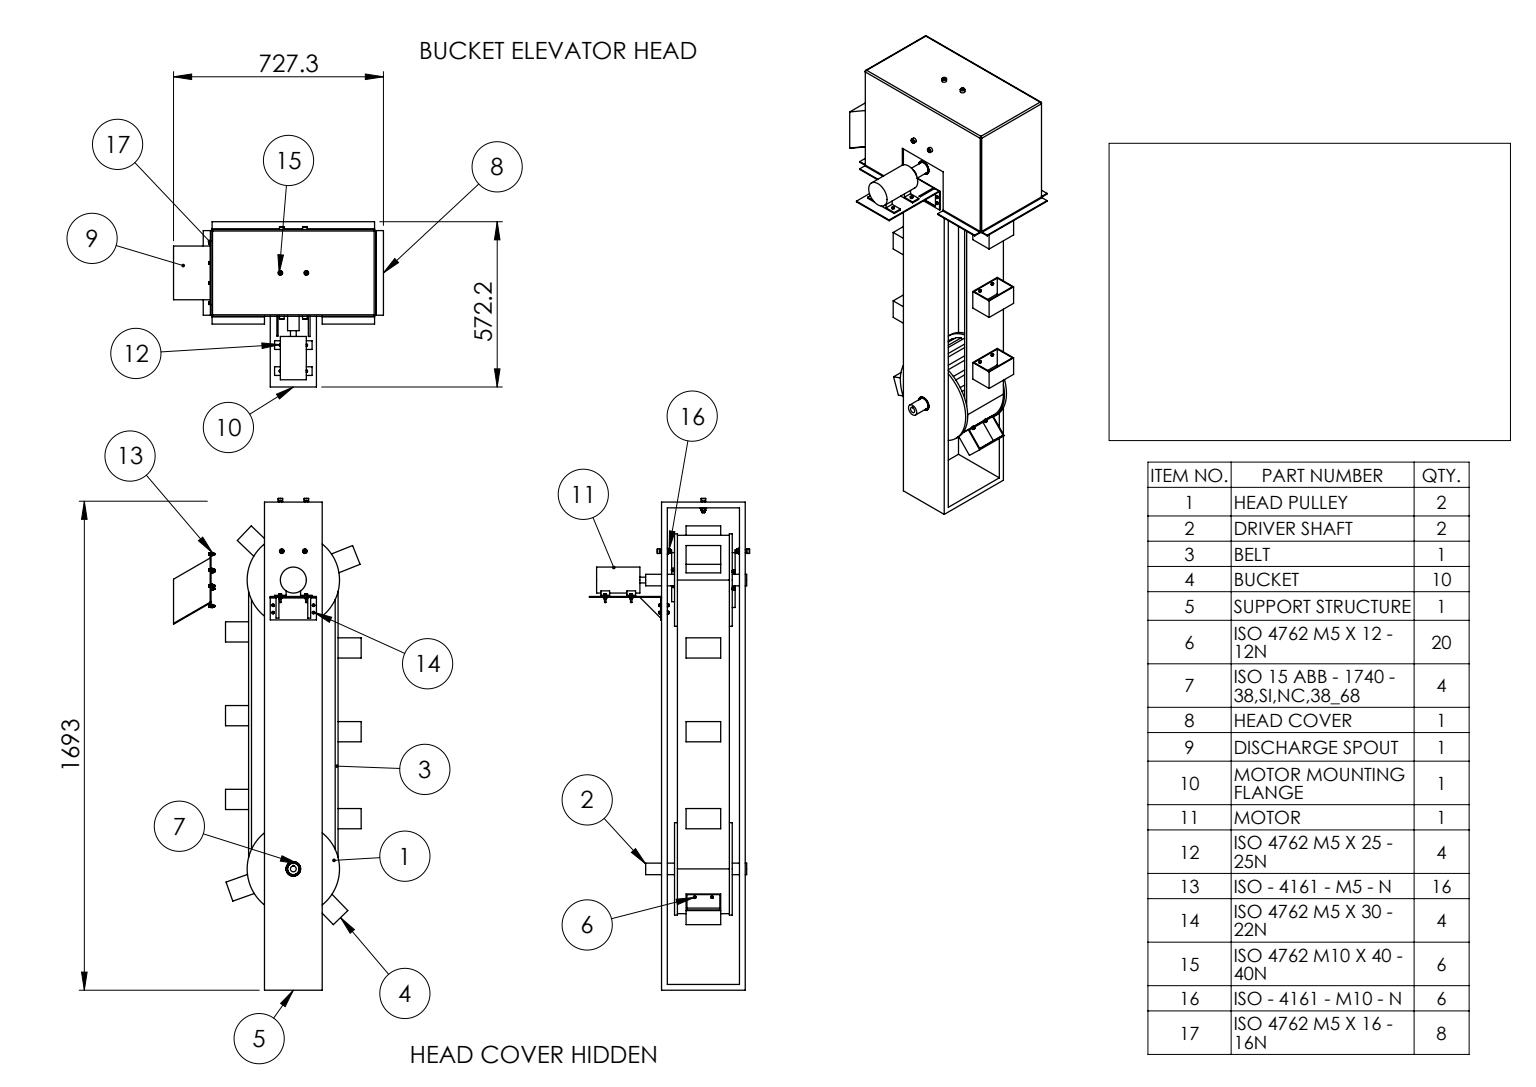
ISO-10303-21;
HEADER;
FILE_DESCRIPTION (('STEP AP214'),
    '1' );
FILE_NAME ('MAS-186',
    '2026-10-31T03:46:07',
    ( '' ),
    ( '' ),
    'SwSTEP 2.0',
    'SolidWorks 2026',
    '' );
FILE_SCHEMA (( 'AUTOMOTIVE_DESIGN' ));
ENDSEC;

DATA;
#1 = DIRECTION ( 'NONE',  ( -0.000000000000000000, -0.000000000000000000, -1.000000000000000000 ) ) ;
#2 = AXIS2_PLACEMENT_3D ( 'NONE', #6782, #12036, #15971 ) ;
#3 = VECTOR ( 'NONE', #6324, 1000.000000000000000 ) ;
#4 = CIRCLE ( 'NONE', #6942, 9.999999999999998224 ) ;
#5 = EDGE_LOOP ( 'NONE', ( #366, #3432, #8701, #5871, #3805 ) ) ;
#6 = CARTESIAN_POINT ( 'NONE',  ( 18.83467029480910071, -16.52066876451827326, 145.0000119999999697 ) ) ;
#7 = VECTOR ( 'NONE', #7349, 1000.000000000000000 ) ;
#8 = UNCERTAINTY_MEASURE_WITH_UNIT (LENGTH_MEASURE( 1.000000000000000082E-05 ), #17225, 'distance_accuracy_value', 'NONE');
#9 = CARTESIAN_POINT ( 'NONE',  ( 155.0000000000000568, -1000.000000000000000, 90.00000000000000000 ) ) ;
#10 = CARTESIAN_POINT ( 'NONE',  ( 4.000000000000000000, 2.309401076758515803, -0.4999999999999995559 ) ) ;
#11 = AXIS2_PLACEMENT_3D ( 'NONE', #10310, #5106, #19826 ) ;
#12 = VERTEX_POINT ( 'NONE', #4836 ) ;
#13 =( REPRESENTATION_RELATIONSHIP ('NONE','NONE', #10127, #5587 ) REPRESENTATION_RELATIONSHIP_WITH_TRANSFORMATION ( #17180 )SHAPE_REPRESENTATION_RELATIONSHIP( ) );
#14 = DIRECTION ( 'NONE',  ( 1.000000000000000000, -6.640089860198304064E-16, -0.000000000000000000 ) ) ;
#15 = AXIS2_PLACEMENT_3D ( 'NONE', #6057, #12994, #3756 ) ;
#16 = VECTOR ( 'NONE', #9447, 1000.000000000000114 ) ;
#17 = AXIS2_PLACEMENT_3D ( 'NONE', #8698, #6875, #2876 ) ;
#18 = CIRCLE ( 'NONE', #21621, 2.499999999999998668 ) ;
#19 = EDGE_CURVE ( 'NONE', #8380, #2021, #17168, .T. ) ;
#20 = ORIENTED_EDGE ( 'NONE', *, *, #18012, .T. ) ;
#21 = CARTESIAN_POINT ( 'NONE',  ( -31.74999999999995737, 0.000000000000000000, 4.250000000000000000 ) ) ;
#22 = EDGE_CURVE ( 'NONE', #12572, #17693, #16078, .T. ) ;
#23 = DIRECTION ( 'NONE',  ( -0.000000000000000000, -0.000000000000000000, 1.000000000000000000 ) ) ;
#24 = ORIENTED_EDGE ( 'NONE', *, *, #13771, .T. ) ;
#25 = CARTESIAN_POINT ( 'NONE',  ( -128.2695163047654319, 87.01699568756248482, -27.57873596473009670 ) ) ;
#26 = EDGE_CURVE ( 'NONE', #18313, #7126, #7119, .T. ) ;
#27 = DIRECTION ( 'NONE',  ( 0.000000000000000000, 1.177509268541832635E-16, -1.000000000000000000 ) ) ;
#28 = CARTESIAN_POINT ( 'NONE',  ( 15.24974479720505549, -1019.877690639539310, 145.0000119999999697 ) ) ;
#29 = DIRECTION ( 'NONE',  ( 0.000000000000000000, 0.7071067811865489050, 0.7071067811865462405 ) ) ;
#30 = CARTESIAN_POINT ( 'NONE',  ( -3.096526599377909417, 6.872473572140716414, 1.143494478793305063E-15 ) ) ;
#31 = EDGE_CURVE ( 'NONE', #18619, #12627, #9184, .T. ) ;
#32 = EDGE_CURVE ( 'NONE', #16311, #19722, #7366, .T. ) ;
#33 = DIRECTION ( 'NONE',  ( -1.000000000000000000, -0.000000000000000000, -0.000000000000000000 ) ) ;
#34 = EDGE_LOOP ( 'NONE', ( #18835, #10262, #758, #19921 ) ) ;
#23804 = DIRECTION ( 'NONE',  ( -1.000000000000000000, -0.000000000000000000, -0.000000000000000000 ) ) ;
#36 = CARTESIAN_POINT ( 'NONE',  ( -146.0000000000001137, -204.4690652294807478, 27.94500000000641649 ) ) ;
#37 = LINE ( 'NONE', #254, #11884 ) ;
#38 = SURFACE_SIDE_STYLE ('',( #3514 ) ) ;
#39 = VECTOR ( 'NONE', #3560, 1000.000000000000000 ) ;
#41 = ORIENTED_EDGE ( 'NONE', *, *, #15976, .F. ) ;
#40 = EDGE_LOOP ( 'NONE', ( #2219, #256, #14388 ) ) ;
#42 = DIRECTION ( 'NONE',  ( 1.000000000000000000, 0.000000000000000000, 0.000000000000000000 ) ) ;
#43 = CARTESIAN_POINT ( 'NONE',  ( 0.000000000000000000, 1.178949249685218970, 2.041999999999998483 ) ) ;
#44 = CARTESIAN_POINT ( 'NONE',  ( 280.4976310729377929, 269.6958543268122526, -146.0927021017107279 ) ) ;
#45 = VERTEX_POINT ( 'NONE', #9 ) ;
#46 = DIRECTION ( 'NONE',  ( 1.000000000000000000, -0.000000000000000000, -0.000000000000000000 ) ) ;
#47 = EDGE_LOOP ( 'NONE', ( #6115, #19407 ) ) ;
#48 = CARTESIAN_POINT ( 'NONE',  ( 80.00000000000004263, -137.9999999999999716, 3.000000000000000000 ) ) ;
#49 = ORIENTED_EDGE ( 'NONE', *, *, #7796, .F. ) ;
#50 = CARTESIAN_POINT ( 'NONE',  ( 281.4928932188134354, -129.2000000000000455, -150.2000000000013245 ) ) ;
#51 = DIRECTION ( 'NONE',  ( -0.000000000000000000, 3.469446951953613794E-15, 1.000000000000000000 ) ) ;
#52 = VERTEX_POINT ( 'NONE', #18122 ) ;
#53 = LINE ( 'NONE', #5589, #20648 ) ;
#54 = EDGE_LOOP ( 'NONE', ( #6384, #11170, #16002, #7000 ) ) ;
#55 = DIRECTION ( 'NONE',  ( 0.9289202219288174023, 0.3702799228849934510, 6.982962677686266711E-15 ) ) ;
#56 = CARTESIAN_POINT ( 'NONE',  ( 133.4872637682705090, 78.77924338079024835, 32.17229779615544771 ) ) ;
#57 = CARTESIAN_POINT ( 'NONE',  ( 3.511755186886750923, -2.826662030176382956, -3.597382984111582083 ) ) ;
#58 = DIRECTION ( 'NONE',  ( -1.000000000000000000, 0.000000000000000000, 0.000000000000000000 ) ) ;
#59 = EDGE_CURVE ( 'NONE', #14664, #1301, #12963, .T. ) ;
#60 = EDGE_CURVE ( 'NONE', #21739, #840, #11018, .T. ) ;
#61 = CARTESIAN_POINT ( 'NONE',  ( -4.204015924366189871, 1.626724848190922446, -3.610627190413390419 ) ) ;
#62 = EDGE_CURVE ( 'NONE', #22159, #2544, #22076, .T. ) ;
#63 = ORIENTED_EDGE ( 'NONE', *, *, #22259, .T. ) ;
#64 = DIRECTION ( 'NONE',  ( 0.000000000000000000, 0.000000000000000000, 1.000000000000000000 ) ) ;
#65 = CARTESIAN_POINT ( 'NONE',  ( -7.500000000000000000, 4.330127018922191873, -0.9999999999999970024 ) ) ;
#66 = CARTESIAN_POINT ( 'NONE',  ( 1.249999999999999112, -7.938566201357367902, -7.198902722707431145 ) ) ;
#67 = VERTEX_POINT ( 'NONE', #12958 ) ;
#68 = CARTESIAN_POINT ( 'NONE',  ( 281.3673618604586295, 268.0905802150185195, -147.1999999999998749 ) ) ;
#69 = CARTESIAN_POINT ( 'NONE',  ( 107.6499999999999631, -19.99999999999998934, 0.000000000000000000 ) ) ;
#70 = CARTESIAN_POINT ( 'NONE',  ( 7.499999999999999112, 0.7513028741560161539, -0.02472015219302839059 ) ) ;
#71 = DIRECTION ( 'NONE',  ( 1.000000000000000000, 0.000000000000000000, 0.000000000000000000 ) ) ;
#72 = CARTESIAN_POINT ( 'NONE',  ( 5.000000000000002665, 0.000000000000000000, -2.700000000000000622 ) ) ;
#73 = ORIENTED_EDGE ( 'NONE', *, *, #3413, .T. ) ;
#74 = CARTESIAN_POINT ( 'NONE',  ( 126.3653543294811499, 77.28387428943223370, 30.00000000000641620 ) ) ;
#75 = ORIENTED_EDGE ( 'NONE', *, *, #4902, .T. ) ;
#76 = CARTESIAN_POINT ( 'NONE',  ( 3.333333333333335702, -2.694301256218268215, -3.300726591567084256 ) ) ;
#77 = CARTESIAN_POINT ( 'NONE',  ( -69.99999999999997158, -87.33333333333338544, 145.0000000000000000 ) ) ;
#78 = LINE ( 'NONE', #5499, #566 ) ;
#79 = ORIENTED_EDGE ( 'NONE', *, *, #18426, .F. ) ;
#80 = DIRECTION ( 'NONE',  ( -0.000000000000000000, 1.287488025362403787E-15, 1.000000000000000000 ) ) ;
#81 = DIRECTION ( 'NONE',  ( 1.000000000000000000, 0.000000000000000000, 0.000000000000000000 ) ) ;
#82 = LINE ( 'NONE', #14822, #8863 ) ;
#83 = FACE_OUTER_BOUND ( 'NONE', #5048, .T. ) ;
#84 = EDGE_CURVE ( 'NONE', #20571, #4595, #14131, .T. ) ;
#85 = DIRECTION ( 'NONE',  ( 0.000000000000000000, 0.000000000000000000, 1.000000000000000000 ) ) ;
#86 = DIRECTION ( 'NONE',  ( 1.000000000000000000, 0.000000000000000000, 0.000000000000000000 ) ) ;
#87 = DIRECTION ( 'NONE',  ( -1.000000000000000000, -0.000000000000000000, -0.000000000000000000 ) ) ;
#88 = ADVANCED_FACE ( 'NONE', ( #16201 ), #18340, .T. ) ;
#89 = ORIENTED_EDGE ( 'NONE', *, *, #1676, .F. ) ;
#90 = EDGE_LOOP ( 'NONE', ( #21123, #7756, #684, #7867 ) ) ;
#91 = CARTESIAN_POINT ( 'NONE',  ( -2.688821387764050996E-14, -4.618802153517012954, -0.4999999999999995559 ) ) ;
#92 = DIRECTION ( 'NONE',  ( 1.000000000000000000, 0.000000000000000000, 0.000000000000000000 ) ) ;
#93 = ORIENTED_EDGE ( 'NONE', *, *, #8723, .F. ) ;
#94 = PLANE ( 'NONE',  #21616 ) ;
#95 = CARTESIAN_POINT ( 'NONE',  ( -0.2779000157839473517, -8.820699686765063774, -7.928862157988305626 ) ) ;
#96 = CARTESIAN_POINT ( 'NONE',  ( 0.000000000000000000, -1000.000000000000000, 138.9999999999999716 ) ) ;
#97 = ORIENTED_EDGE ( 'NONE', *, *, #11862, .T. ) ;
#98 = CARTESIAN_POINT ( 'NONE',  ( 110.0000000000000000, 95.00000000000000000, 3.000000000000000000 ) ) ;
#99 = DIRECTION ( 'NONE',  ( -1.000000000000000000, -0.000000000000000000, -0.000000000000000000 ) ) ;
#100 = DIRECTION ( 'NONE',  ( 0.000000000000000000, 0.000000000000000000, 1.000000000000000000 ) ) ;
#101 = ORIENTED_EDGE ( 'NONE', *, *, #6605, .F. ) ;
#102 = CARTESIAN_POINT ( 'NONE',  ( 100.0000000000000000, 249.9999999999999716, 125.0000000000000284 ) ) ;
#103 = DIRECTION ( 'NONE',  ( 1.000000000000000000, 0.000000000000000000, 0.000000000000000000 ) ) ;
#104 = DIRECTION ( 'NONE',  ( 0.4924295582441756136, -0.5074575156280946020, -0.7071067811865532349 ) ) ;
#105 = ORIENTED_EDGE ( 'NONE', *, *, #5663, .T. ) ;
#106 = ORIENTED_EDGE ( 'NONE', *, *, #18345, .F. ) ;
#107 = EDGE_CURVE ( 'NONE', #20023, #9785, #19883, .T. ) ;
#108 = LINE ( 'NONE', #2015, #19648 ) ;
#109 = AXIS2_PLACEMENT_3D ( 'NONE', #8463, #1435, #15716 ) ;
#110 = SHAPE_DEFINITION_REPRESENTATION ( #7281, #4815 ) ;
#111 = CARTESIAN_POINT ( 'NONE',  ( -127.8094121079449081, 87.69139705313254751, -27.49999999999350919 ) ) ;
#112 = DIRECTION ( 'NONE',  ( 1.302872740555339390E-32, -4.694093751100962712E-16, 1.000000000000000000 ) ) ;
#113 = CYLINDRICAL_SURFACE ( 'NONE', #13258, 2.500000000000002220 ) ;
#114 = ORIENTED_EDGE ( 'NONE', *, *, #423, .T. ) ;
#115 = CARTESIAN_POINT ( 'NONE',  ( -11.07878015919984982, -22.47082401081930669, 145.0000119999999697 ) ) ;
#116 = EDGE_CURVE ( 'NONE', #3375, #7169, #11833, .T. ) ;
#117 = ADVANCED_FACE ( 'NONE', ( #14863 ), #10660, .T. ) ;
#118 = ORIENTED_EDGE ( 'NONE', *, *, #9891, .T. ) ;
#119 = DIRECTION ( 'NONE',  ( 1.000000000000000000, 0.000000000000000000, 0.000000000000000000 ) ) ;
#120 = LINE ( 'NONE', #7470, #18771 ) ;
#121 = ORIENTED_EDGE ( 'NONE', *, *, #12195, .F. ) ;
#122 = DIRECTION ( 'NONE',  ( -1.000000000000000000, 3.051161311199799893E-31, 8.144298233840332611E-17 ) ) ;
#123 = ORIENTED_EDGE ( 'NONE', *, *, #13032, .T. ) ;
#124 = CARTESIAN_POINT ( 'NONE',  ( 2.500000000000000000, -1.178949249685214307, 2.042000000000001592 ) ) ;
#125 = DIRECTION ( 'NONE',  ( 0.000000000000000000, 0.000000000000000000, 1.000000000000000000 ) ) ;
#126 = ORIENTED_EDGE ( 'NONE', *, *, #10672, .T. ) ;
#127 = CARTESIAN_POINT ( 'NONE',  ( 2.500000000000000000, 1.178949249685213863, -2.042000000000001148 ) ) ;
#128 = CARTESIAN_POINT ( 'NONE',  ( 281.4928932188134354, -132.2000000000000455, -177.2000000000013529 ) ) ;
#129 = AXIS2_PLACEMENT_3D ( 'NONE', #9738, #17091, #22629 ) ;
#130 = FACE_BOUND ( 'NONE', #10121, .T. ) ;
#131 = CARTESIAN_POINT ( 'NONE',  ( 284.6730547946947354, 270.1059783239180661, 146.0571358042176087 ) ) ;
#132 = AXIS2_PLACEMENT_3D ( 'NONE', #19134, #13752, #799 ) ;
#133 =( REPRESENTATION_RELATIONSHIP ('NONE','NONE', #10127, #14711 ) REPRESENTATION_RELATIONSHIP_WITH_TRANSFORMATION ( #8264 )SHAPE_REPRESENTATION_RELATIONSHIP( ) );
#134 = CARTESIAN_POINT ( 'NONE',  ( -91.18044947428953151, 112.7436279071528702, 90.00000000000000000 ) ) ;
#135 = ADVANCED_FACE ( 'NONE', ( #19802 ), #12982, .T. ) ;
#136 = DIRECTION ( 'NONE',  ( -1.000000000000000000, -0.000000000000000000, -0.000000000000000000 ) ) ;
#137 = ORIENTED_EDGE ( 'NONE', *, *, #23350, .T. ) ;
#138 = ADVANCED_FACE ( 'NONE', ( #8828 ), #23557, .F. ) ;
#139 = FACE_BOUND ( 'NONE', #47, .T. ) ;
#140 = FACE_BOUND ( 'NONE', #2354, .T. ) ;
#142 = ORIENTED_EDGE ( 'NONE', *, *, #15816, .T. ) ;
#141 = ORIENTED_EDGE ( 'NONE', *, *, #17752, .T. ) ;
#143 = CARTESIAN_POINT ( 'NONE',  ( -69.99999999999998579, -87.33333333333338544, 119.9999999999999716 ) ) ;
#144 = CARTESIAN_POINT ( 'NONE',  ( -136.7455495141632014, -1072.977142426286946, -31.53250949154617189 ) ) ;
#145 = CARTESIAN_POINT ( 'NONE',  ( 5.200000000000002842, 0.000000000000000000, 0.000000000000000000 ) ) ;
#146 = ADVANCED_FACE ( 'NONE', ( #21970 ), #14402, .F. ) ;
#147 = ORIENTED_EDGE ( 'NONE', *, *, #7523, .T. ) ;
#148 = CIRCLE ( 'NONE', #12147, 2.700000000000000622 ) ;
#149 = EDGE_CURVE ( 'NONE', #7198, #16229, #4462, .T. ) ;
#150 = CARTESIAN_POINT ( 'NONE',  ( -134.5566256099404825, -1076.938388239963842, 30.33200430454444785 ) ) ;
#151 = ORIENTED_EDGE ( 'NONE', *, *, #12197, .F. ) ;
#152 = DIRECTION ( 'NONE',  ( 0.000000000000000000, 0.000000000000000000, -1.000000000000000000 ) ) ;
#153 = ADVANCED_FACE ( 'NONE', ( #23660 ), #11773, .F. ) ;
#154 = ORIENTED_EDGE ( 'NONE', *, *, #8010, .T. ) ;
#155 = DIRECTION ( 'NONE',  ( -0.000000000000000000, 0.000000000000000000, 1.000000000000000000 ) ) ;
#156 = CARTESIAN_POINT ( 'NONE',  ( 5.000000000000015099, 0.000000000000000000, 0.000000000000000000 ) ) ;
#157 = EDGE_CURVE ( 'NONE', #8899, #17134, #9062, .T. ) ;
#158 = EDGE_LOOP ( 'NONE', ( #17391, #12843, #343, #3950 ) ) ;
#159 = CARTESIAN_POINT ( 'NONE',  ( 125.5946212300931251, -1090.835042168281007, 31.66065886938999796 ) ) ;
#160 = VERTEX_POINT ( 'NONE', #20384 ) ;
#161 = CARTESIAN_POINT ( 'NONE',  ( -129.3084827928275899, 85.46529914716332144, 30.33200430454444785 ) ) ;
#162 = CARTESIAN_POINT ( 'NONE',  ( 4.999999999999999112, 5.773502691896256422, -7.063244554129997965 ) ) ;
#163 = DIRECTION ( 'NONE',  ( 1.000000000000000000, 0.000000000000000000, 0.000000000000000000 ) ) ;
#164 = PRESENTATION_LAYER_ASSIGNMENT (  '', '', ( #545 ) ) ;
#165 = CIRCLE ( 'NONE', #9426, 5.249999999999949374 ) ;
#166 = FACE_OUTER_BOUND ( 'NONE', #524, .T. ) ;
#167 = DIRECTION ( 'NONE',  ( 0.000000000000000000, 0.000000000000000000, -1.000000000000000000 ) ) ;
#168 = VECTOR ( 'NONE', #12826, 1000.000000000000000 ) ;
#169 = ORIENTED_EDGE ( 'NONE', *, *, #10857, .T. ) ;
#170 = B_SPLINE_CURVE_WITH_KNOTS ( 'NONE', 3,
 ( #22399, #16491, #3559, #1745, #10973, #23729, #1990, #12913, #5622, #7185, #14575, #13162, #16380, #9267, #21916, #7319, #18537, #13033, #1867, #10867, #14821, #16628, #20334, #18294, #9136, #12812, #18638, #15068, #11086, #11248, #14938, #14705 ),
 .UNSPECIFIED., .F., .F.,
 ( 4, 2, 2, 2, 2, 2, 2, 2, 2, 2, 2, 2, 2, 2, 2, 4 ),
 ( 1.551583845779545699E-17, 0.0004914281572964048763, 0.0009828563145927943570, 0.001474284471889183512, 0.001965712629185573102, 0.002457140786481962474, 0.002948568943778351412, 0.003931425258371110641, 0.004422853415667485702, 0.004914281572963859895, 0.005405709730260234956, 0.005897137887556608282, 0.006388566044852983343, 0.006879994202149357536, 0.007371422359445732597, 0.007862850516742106791 ),
 .UNSPECIFIED. ) ;
#171 = EDGE_CURVE ( 'NONE', #22518, #4872, #9420, .T. ) ;
#172 = LINE ( 'NONE', #13494, #7239 ) ;
#173 = CARTESIAN_POINT ( 'NONE',  ( 131.5154891841473841, 82.02850787876496952, -30.32849798811265885 ) ) ;
#174 = ADVANCED_FACE ( 'NONE', ( #20884 ), #9674, .F. ) ;
#175 = ORIENTED_EDGE ( 'NONE', *, *, #23587, .F. ) ;
#176 = DIRECTION ( 'NONE',  ( -1.000000000000000000, -0.000000000000000000, -0.000000000000000000 ) ) ;
#177 = CARTESIAN_POINT ( 'NONE',  ( -34.75000000000005684, 100.0000000000000000, 150.2000000000009550 ) ) ;
#178 = AXIS2_PLACEMENT_3D ( 'NONE', #20566, #18993, #2455 ) ;
#179 = EDGE_CURVE ( 'NONE', #21239, #21516, #2397, .T. ) ;
#180 = DIRECTION ( 'NONE',  ( 0.000000000000000000, 0.000000000000000000, 1.000000000000000000 ) ) ;
#181 = AXIS2_PLACEMENT_3D ( 'NONE', #11379, #9543, #20890 ) ;
#182 = ADVANCED_FACE ( 'NONE', ( #22679 ), #11370, .F. ) ;
#183 = EDGE_CURVE ( 'NONE', #1893, #16800, #2084, .T. ) ;
#184 = DIRECTION ( 'NONE',  ( 0.000000000000000000, -1.000000000000000000, 0.000000000000000000 ) ) ;
#185 = EDGE_CURVE ( 'NONE', #19310, #4045, #11744, .T. ) ;
#186 = DIRECTION ( 'NONE',  ( 0.000000000000000000, 0.000000000000000000, 1.000000000000000000 ) ) ;
#187 = ORIENTED_EDGE ( 'NONE', *, *, #21854, .T. ) ;
#188 = PRESENTATION_LAYER_ASSIGNMENT (  '', '', ( #17925 ) ) ;
#189 = DIRECTION ( 'NONE',  ( 0.9289202219288174023, 0.3702799228849934510, 6.982962677686266711E-15 ) ) ;
#190 = ORIENTED_EDGE ( 'NONE', *, *, #703, .F. ) ;
#191 = VECTOR ( 'NONE', #8346, 999.9999999999998863 ) ;
#192 = DIRECTION ( 'NONE',  ( -0.9289202219288174023, -0.3702799228849933955, -6.982962677686267499E-15 ) ) ;
#193 = DIRECTION ( 'NONE',  ( 0.000000000000000000, 1.177509268541832635E-16, -1.000000000000000000 ) ) ;
#194 = DIRECTION ( 'NONE',  ( -0.000000000000000000, -0.000000000000000000, -1.000000000000000000 ) ) ;
#195 = EDGE_LOOP ( 'NONE', ( #21497, #11165, #16158, #18596 ) ) ;
#196 = CARTESIAN_POINT ( 'NONE',  ( 0.000000000000000000, 0.000000000000000000, 0.000000000000000000 ) ) ;
#197 = LINE ( 'NONE', #22401, #4609 ) ;
#198 = DIRECTION ( 'NONE',  ( 3.469446951953614682E-16, -1.000000000000000000, 3.483493295888648978E-15 ) ) ;
#199 = DIRECTION ( 'NONE',  ( -0.000000000000000000, -0.000000000000000000, 1.000000000000000000 ) ) ;
#200 = CARTESIAN_POINT ( 'NONE',  ( 2.500000000000000000, -2.357898499370432166, 3.035766082959412415E-15 ) ) ;
#201 = CARTESIAN_POINT ( 'NONE',  ( -7.500000000000000000, -4.732323933430407692, -7.493854309896101462 ) ) ;
#202 = CIRCLE ( 'NONE', #14864, 2.649999999999971934 ) ;
#203 = ORIENTED_EDGE ( 'NONE', *, *, #11821, .T. ) ;
#204 = CARTESIAN_POINT ( 'NONE',  ( 194.7499999999997442, -209.9999999999996874, 30.00000000000675726 ) ) ;
#205 = CARTESIAN_POINT ( 'NONE',  ( 2.500000000000000444, 0.000000000000000000, -25.03750572909317285 ) ) ;
#206 = ORIENTED_EDGE ( 'NONE', *, *, #14942, .F. ) ;
#207 = AXIS2_PLACEMENT_3D ( 'NONE', #19783, #10642, #8811 ) ;
#208 = DIRECTION ( 'NONE',  ( -1.350636282998972974E-14, 0.000000000000000000, -1.000000000000000000 ) ) ;
#209 = DIRECTION ( 'NONE',  ( 3.469446951953614682E-16, -1.000000000000000000, 3.491481338843133355E-15 ) ) ;
#210 = CARTESIAN_POINT ( 'NONE',  ( 281.1021437883072167, 269.7094021484633686, -145.4974534559949859 ) ) ;
#211 = EDGE_LOOP ( 'NONE', ( #6410, #3286, #15490, #21044 ) ) ;
#212 = ADVANCED_FACE ( 'NONE', ( #22806 ), #18937, .T. ) ;
#213 = CIRCLE ( 'NONE', #14875, 160.0000000000000000 ) ;
#214 = FACE_BOUND ( 'NONE', #6282, .T. ) ;
#215 = EDGE_CURVE ( 'NONE', #12818, #8899, #13572, .T. ) ;
#216 = CARTESIAN_POINT ( 'NONE',  ( -6.127431526422343306E-17, 9.147862274876549904, -8.047472243342932430 ) ) ;
#217 = CARTESIAN_POINT ( 'NONE',  ( 0.000000000000000000, 0.000000000000000000, 90.00000000000000000 ) ) ;
#218 = VERTEX_POINT ( 'NONE', #2274 ) ;
#219 = EDGE_CURVE ( 'NONE', #14233, #9344, #13241, .T. ) ;
#220 = CARTESIAN_POINT ( 'NONE',  ( 2.999999999999995559, 2.574819895207310198E-15, 21.02499999999999858 ) ) ;
#221 = CARTESIAN_POINT ( 'NONE',  ( -135.9481979339306577, -1074.452087582500553, 27.51597717546056643 ) ) ;
#222 = CARTESIAN_POINT ( 'NONE',  ( -6.259644161404862988E-16, -4.618802153517027165, -3.504271511726793076 ) ) ;
#223 = VERTEX_POINT ( 'NONE', #18684 ) ;
#224 = DIRECTION ( 'NONE',  ( 0.000000000000000000, -1.000000000000000000, -1.177509268541832635E-16 ) ) ;
#225 = VECTOR ( 'NONE', #9857, 1000.000000000000000 ) ;
#226 = PRODUCT_CONTEXT ( 'NONE', #16017, 'mechanical' ) ;
#227 = VECTOR ( 'NONE', #939, 1000.000000000000000 ) ;
#228 = CARTESIAN_POINT ( 'NONE',  ( -44.99999999999995026, -52.79999999999969873, 50.00000000000018474 ) ) ;
#229 = DIRECTION ( 'NONE',  ( 0.000000000000000000, 0.000000000000000000, 1.000000000000000000 ) ) ;
#230 = CARTESIAN_POINT ( 'NONE',  ( 0.2500000000000002220, 0.000000000000000000, 0.000000000000000000 ) ) ;
#231 = ORIENTED_EDGE ( 'NONE', *, *, #16834, .F. ) ;
#232 = EDGE_LOOP ( 'NONE', ( #16649, #15723, #18721 ) ) ;
#233 = LINE ( 'NONE', #3596, #6438 ) ;
#234 = AXIS2_PLACEMENT_3D ( 'NONE', #5498, #20216, #1399 ) ;
#235 = AXIS2_PLACEMENT_3D ( 'NONE', #16320, #23663, #13576 ) ;
#236 = AXIS2_PLACEMENT_3D ( 'NONE', #4373, #19210, #636 ) ;
#237 = DIRECTION ( 'NONE',  ( 0.000000000000000000, -1.000000000000000000, 0.000000000000000000 ) ) ;
#238 = CARTESIAN_POINT ( 'NONE',  ( 2.500000000000000000, 2.357898499370432166, -2.385244779468109755E-15 ) ) ;
#239 = EDGE_LOOP ( 'NONE', ( #13471, #13431, #11953, #18524 ) ) ;
#240 = DIRECTION ( 'NONE',  ( 0.000000000000000000, 0.000000000000000000, -1.000000000000000000 ) ) ;
#241 = EDGE_CURVE ( 'NONE', #17193, #16244, #10661, .T. ) ;
#242 = ORIENTED_EDGE ( 'NONE', *, *, #6175, .T. ) ;
#243 = DIRECTION ( 'NONE',  ( 1.000000000000000000, 0.000000000000000000, 0.000000000000000000 ) ) ;
#244 = DIRECTION ( 'NONE',  ( 1.000000000000000000, -0.000000000000000000, -0.000000000000000000 ) ) ;
#245 = EDGE_LOOP ( 'NONE', ( #12750, #13760, #3479, #23001 ) ) ;
#246 = CARTESIAN_POINT ( 'NONE',  ( -0.6508621380849236582, -8.763657152406455708, -7.907633014911225722 ) ) ;
#247 = CYLINDRICAL_SURFACE ( 'NONE', #10836, 20.00000000000000000 ) ;
#248 = CARTESIAN_POINT ( 'NONE',  ( 37.64999999999997726, 90.00000000000000000, 3.000000000000001332 ) ) ;
#249 = CARTESIAN_POINT ( 'NONE',  ( -100.0000000000000000, 35.00000000000009948, 150.2000000000008413 ) ) ;
#250 = DIRECTION ( 'NONE',  ( -0.000000000000000000, -0.000000000000000000, -1.000000000000000000 ) ) ;
#251 = CARTESIAN_POINT ( 'NONE',  ( 2.171643655288379993, -3.365003104552334978, -1.195831703456429434E-14 ) ) ;
#252 = ORIENTED_EDGE ( 'NONE', *, *, #20392, .F. ) ;
#253 = CARTESIAN_POINT ( 'NONE',  ( 2.500000000000000000, -1.178949249685218748, -2.041999999999998039 ) ) ;
#254 = CARTESIAN_POINT ( 'NONE',  ( 194.7500000000001705, -210.0000000000003411, -27.49999999999322498 ) ) ;
#255 = PRODUCT_DEFINITION_SHAPE ( 'NONE', 'NONE',  #23890 ) ;
#257 = ORIENTED_EDGE ( 'NONE', *, *, #4493, .F. ) ;
#256 = ORIENTED_EDGE ( 'NONE', *, *, #23484, .F. ) ;
#258 = LINE ( 'NONE', #11397, #17366 ) ;
#259 = VECTOR ( 'NONE', #12873, 1000.000000000000000 ) ;
#260 = CARTESIAN_POINT ( 'NONE',  ( 49.17200000000001836, 0.000000000000000000, 5.000000000000002665 ) ) ;
#261 = AXIS2_PLACEMENT_3D ( 'NONE', #2873, #10278, #8330 ) ;
#262 = ORIENTED_EDGE ( 'NONE', *, *, #21312, .T. ) ;
#263 = DIRECTION ( 'NONE',  ( 1.000000000000000000, 0.000000000000000000, 0.000000000000000000 ) ) ;
#264 = ORIENTED_EDGE ( 'NONE', *, *, #1576, .T. ) ;
#265 = CARTESIAN_POINT ( 'NONE',  ( 280.3431883566700549, 273.0000000000000568, -145.0627246244601167 ) ) ;
#266 = ORIENTED_EDGE ( 'NONE', *, *, #12996, .T. ) ;
#267 = EDGE_CURVE ( 'NONE', #8364, #19016, #14886, .T. ) ;
#268 = LINE ( 'NONE', #7399, #2277 ) ;
#269 = DIRECTION ( 'NONE',  ( -3.469446951953614682E-16, 1.000000000000000000, -3.483493295888648978E-15 ) ) ;
#270 = ADVANCED_FACE ( 'NONE', ( #15223 ), #15473, .F. ) ;
#271 = EDGE_CURVE ( 'NONE', #15472, #22598, #15342, .T. ) ;
#272 = AXIS2_PLACEMENT_3D ( 'NONE', #19856, #3615, #4354 ) ;
#273 = ITEM_DEFINED_TRANSFORMATION ( 'NONE', 'NONE', #18507,  #11210 ) ;
#274 = ORIENTED_EDGE ( 'NONE', *, *, #4252, .F. ) ;
#275 = CARTESIAN_POINT ( 'NONE',  ( 125.1337793500219817, -1091.468903702553689, 27.75096515221187232 ) ) ;
#276 = ORIENTED_EDGE ( 'NONE', *, *, #12482, .T. ) ;
#277 = AXIS2_PLACEMENT_3D ( 'NONE', #7099, #10883, #12700 ) ;
#278 = CARTESIAN_POINT ( 'NONE',  ( -127.9949300873395543, 87.42039156790949050, 32.50000000000647304 ) ) ;
#279 = EDGE_CURVE ( 'NONE', #7198, #16055, #16896, .T. ) ;
#280 = SURFACE_STYLE_USAGE ( .BOTH. , #5947 ) ;
#281 = LINE ( 'NONE', #5839, #17682 ) ;
#282 = CARTESIAN_POINT ( 'NONE',  ( 2.500000000000000000, 1.178949249685213863, -2.042000000000001148 ) ) ;
#283 = ORIENTED_EDGE ( 'NONE', *, *, #21682, .F. ) ;
#284 = CARTESIAN_POINT ( 'NONE',  ( -280.9952621458755857, 268.9079617568159506, -146.9223300543793584 ) ) ;
#285 = PRESENTATION_STYLE_ASSIGNMENT (( #3537 ) ) ;
#286 = VERTEX_POINT ( 'NONE', #17139 ) ;
#287 = B_SPLINE_CURVE_WITH_KNOTS ( 'NONE', 3,
 ( #4125, #526, #13356, #5838, #13245, #20670, #11305, #18611 ),
 .UNSPECIFIED., .F., .F.,
 ( 4, 2, 2, 4 ),
 ( 0.000000000000000000, 0.002450665683189820997, 0.003675998524784731495, 0.004901331366379641993 ),
 .UNSPECIFIED. ) ;
#288 = EDGE_CURVE ( 'NONE', #16653, #6623, #20746, .T. ) ;
#289 = LINE ( 'NONE', #9594, #2999 ) ;
#290 = CARTESIAN_POINT ( 'NONE',  ( 132.6714475832646656, 80.14557597090949059, -27.51562286569268423 ) ) ;
#291 = AXIS2_PLACEMENT_3D ( 'NONE', #21240, #8314, #10626 ) ;
#292 = CARTESIAN_POINT ( 'NONE',  ( 281.8958543268121844, 268.8927021017106540, 145.9952621458756710 ) ) ;
#293 = DIRECTION ( 'NONE',  ( 0.000000000000000000, 0.000000000000000000, -1.000000000000000000 ) ) ;
#294 = AXIS2_PLACEMENT_3D ( 'NONE', #882, #5000, #6440 ) ;
#295 = VECTOR ( 'NONE', #20136, 1000.000000000000000 ) ;
#296 = VECTOR ( 'NONE', #1760, 1000.000000000000000 ) ;
#297 = FACE_OUTER_BOUND ( 'NONE', #16595, .T. ) ;
#298 = LINE ( 'NONE', #3551, #3445 ) ;
#299 = ORIENTED_EDGE ( 'NONE', *, *, #12045, .F. ) ;
#300 = DIRECTION ( 'NONE',  ( 1.000000000000000000, 3.202566417187951028E-16, 6.405132834375902056E-16 ) ) ;
#301 = VERTEX_POINT ( 'NONE', #17262 ) ;
#302 = DIRECTION ( 'NONE',  ( 0.000000000000000000, 0.000000000000000000, -1.000000000000000000 ) ) ;
#303 =( NAMED_UNIT ( * ) PLANE_ANGLE_UNIT ( ) SI_UNIT ( $, .RADIAN. ) );
#304 = DIRECTION ( 'NONE',  ( -1.000000000000000000, -0.000000000000000000, 0.000000000000000000 ) ) ;
#305 = EDGE_CURVE ( 'NONE', #16453, #7964, #16042, .T. ) ;
#306 = VERTEX_POINT ( 'NONE', #2634 ) ;
#307 = AXIS2_PLACEMENT_3D ( 'NONE', #11338, #18648, #9749 ) ;
#308 = DIRECTION ( 'NONE',  ( 0.000000000000000000, 0.000000000000000000, -1.000000000000000000 ) ) ;
#309 = LINE ( 'NONE', #9020, #16498 ) ;
#310 = EDGE_CURVE ( 'NONE', #18225, #10909, #8683, .T. ) ;
#311 = CARTESIAN_POINT ( 'NONE',  ( 2.500000000000000000, -1.178949249685214307, 2.042000000000001592 ) ) ;
#312 = DIRECTION ( 'NONE',  ( 0.000000000000000000, -1.000000000000000000, 0.000000000000000000 ) ) ;
#313 = EDGE_CURVE ( 'NONE', #14070, #15403, #21354, .T. ) ;
#314 = AXIS2_PLACEMENT_3D ( 'NONE', #11031, #20164, #12506 ) ;
#315 = DIRECTION ( 'NONE',  ( 0.000000000000000000, 0.000000000000000000, 1.000000000000000000 ) ) ;
#316 = CARTESIAN_POINT ( 'NONE',  ( 4.211140560182196957, 2.431303136016536470, -3.745885042887433514 ) ) ;
#317 = AXIS2_PLACEMENT_3D ( 'NONE', #22768, #2356, #2723 ) ;
#318 = DIRECTION ( 'NONE',  ( 0.000000000000000000, 0.000000000000000000, -1.000000000000000000 ) ) ;
#319 = AXIS2_PLACEMENT_3D ( 'NONE', #13284, #11460, #20592 ) ;
#320 = EDGE_CURVE ( 'NONE', #20633, #11416, #17854, .T. ) ;
#321 = VERTEX_POINT ( 'NONE', #4698 ) ;
#322 = ADVANCED_FACE ( 'NONE', ( #4811 ), #10520, .T. ) ;
#323 = CYLINDRICAL_SURFACE ( 'NONE', #9568, 2.500000000000002220 ) ;
#324 = DIRECTION ( 'NONE',  ( 0.000000000000000000, 0.000000000000000000, 1.000000000000000000 ) ) ;
#325 = ADVANCED_FACE ( 'NONE', ( #8567 ), #12223, .F. ) ;
#326 = VERTEX_POINT ( 'NONE', #2863 ) ;
#327 = VERTEX_POINT ( 'NONE', #10267 ) ;
#328 = DIRECTION ( 'NONE',  ( 0.000000000000000000, 0.000000000000000000, 1.000000000000000000 ) ) ;
#329 = DIRECTION ( 'NONE',  ( 1.000000000000000000, 0.000000000000000000, 0.000000000000000000 ) ) ;
#330 = CARTESIAN_POINT ( 'NONE',  ( 5.000000000000000000, 4.685197434473814759, -5.637851296924623057E-15 ) ) ;
#331 = VECTOR ( 'NONE', #4440, 1000.000000000000000 ) ;
#332 = ORIENTED_EDGE ( 'NONE', *, *, #16929, .T. ) ;
#333 = AXIS2_PLACEMENT_3D ( 'NONE', #11581, #4410, #11450 ) ;
#334 = LINE ( 'NONE', #15199, #11800 ) ;
#335 = CARTESIAN_POINT ( 'NONE',  ( 2.500000000000000000, 1.768423874527824902, 1.020999999999999019 ) ) ;
#336 = AXIS2_PLACEMENT_3D ( 'NONE', #12749, #1460, #5215 ) ;
#337 = CARTESIAN_POINT ( 'NONE',  ( -2.617478843592795368, -9.739726766683153514, 200.0000120000000265 ) ) ;
#338 = ORIENTED_EDGE ( 'NONE', *, *, #6400, .F. ) ;
#339 = CARTESIAN_POINT ( 'NONE',  ( 2.500000000000000000, 2.357898499370433054, -1.951563910473907981E-15 ) ) ;
#340 = DIRECTION ( 'NONE',  ( -1.000000000000000000, -0.000000000000000000, -0.000000000000000000 ) ) ;
#341 = AXIS2_PLACEMENT_3D ( 'NONE', #13845, #16102, #21173 ) ;
#342 = CARTESIAN_POINT ( 'NONE',  ( -24.99999999999998224, -1000.000000000000000, -145.0000119999999697 ) ) ;
#343 = ORIENTED_EDGE ( 'NONE', *, *, #12074, .F. ) ;
#344 = CARTESIAN_POINT ( 'NONE',  ( 5.200000000000002842, 0.000000000000000000, 2.500000000000000444 ) ) ;
#345 = SHAPE_DEFINITION_REPRESENTATION ( #14626, #5587 ) ;
#346 = CARTESIAN_POINT ( 'NONE',  ( 34.99999999999999289, 0.000000000000000000, 2.055000000000000160 ) ) ;
#347 = LINE ( 'NONE', #14855, #18432 ) ;
#348 = FACE_OUTER_BOUND ( 'NONE', #9834, .T. ) ;
#349 = ORIENTED_EDGE ( 'NONE', *, *, #18259, .F. ) ;
#350 = AXIS2_PLACEMENT_3D ( 'NONE', #4294, #21542, #12071 ) ;
#352 = ORIENTED_EDGE ( 'NONE', *, *, #7831, .T. ) ;
#351 = ADVANCED_FACE ( 'NONE', ( #21114 ), #3118, .F. ) ;
#353 = EDGE_CURVE ( 'NONE', #6861, #5614, #602, .T. ) ;
#354 = MECHANICAL_DESIGN_GEOMETRIC_PRESENTATION_REPRESENTATION (  '', ( #10787 ), #11568 ) ;
#355 = AXIS2_PLACEMENT_3D ( 'NONE', #12926, #14588, #3930 ) ;
#356 = CARTESIAN_POINT ( 'NONE',  ( 21.69578997558840072, -12.52876685377503740, 145.0000119999999697 ) ) ;
#357 = DIRECTION ( 'NONE',  ( 0.000000000000000000, 0.7071067811865485719, 0.7071067811865465735 ) ) ;
#358 = ADVANCED_FACE ( 'NONE', ( #20999 ), #19173, .F. ) ;
#359 = VECTOR ( 'NONE', #6487, 1000.000000000000000 ) ;
#360 = AXIS2_PLACEMENT_3D ( 'NONE', #12995, #16243, #18159 ) ;
#361 = CIRCLE ( 'NONE', #6148, 2.055000000000001492 ) ;
#362 = PRODUCT_DEFINITION_CONTEXT ( 'detailed design', #17104, 'design' ) ;
#363 = AXIS2_PLACEMENT_3D ( 'NONE', #2805, #6567, #23450 ) ;
#364 = DIRECTION ( 'NONE',  ( 0.000000000000000000, -2.618450529776313049E-15, -1.000000000000000000 ) ) ;
#365 = CARTESIAN_POINT ( 'NONE',  ( -127.2680799365782889, 88.47518962644093676, 27.75040112528346015 ) ) ;
#366 = ORIENTED_EDGE ( 'NONE', *, *, #7485, .F. ) ;
#367 = DIRECTION ( 'NONE',  ( 1.000000000000000000, 0.000000000000000000, -0.000000000000000000 ) ) ;
#368 = EDGE_LOOP ( 'NONE', ( #6453, #4293, #7528, #16012 ) ) ;
#369 = VECTOR ( 'NONE', #13127, 1000.000000000000000 ) ;
#371 = AXIS2_PLACEMENT_3D ( 'NONE', #23355, #14098, #23119 ) ;
#370 =( GEOMETRIC_REPRESENTATION_CONTEXT ( 3 ) GLOBAL_UNCERTAINTY_ASSIGNED_CONTEXT ( ( #3597 ) ) GLOBAL_UNIT_ASSIGNED_CONTEXT ( ( #16013, #5250, #17687 ) ) REPRESENTATION_CONTEXT ( 'NONE', 'WORKASPACE' ) );
#373 = SURFACE_STYLE_USAGE ( .BOTH. , #5673 ) ;
#372 = AXIS2_PLACEMENT_3D ( 'NONE', #12914, #5396, #21586 ) ;
#374 = AXIS2_PLACEMENT_3D ( 'NONE', #18299, #13274, #11090 ) ;
#376 = AXIS2_PLACEMENT_3D ( 'NONE', #537, #9598, #428 ) ;
#375 = DIRECTION ( 'NONE',  ( -0.000000000000000000, 1.000000000000000000, -0.000000000000000000 ) ) ;
#377 = EDGE_LOOP ( 'NONE', ( #20981, #9413, #16535, #22463, #1833 ) ) ;
#378 = EDGE_LOOP ( 'NONE', ( #19734, #5802 ) ) ;
#379 = CARTESIAN_POINT ( 'NONE',  ( 2.742827927723449299, 3.035229711104609596, -3.433252694550591233 ) ) ;
#380 = VECTOR ( 'NONE', #18750, 1000.000000000000114 ) ;
#381 = VECTOR ( 'NONE', #12199, 1000.000000000000000 ) ;
#382 = CARTESIAN_POINT ( 'NONE',  ( -280.4973317504632746, 272.3135885331259374, -147.6045710003933493 ) ) ;
#383 = CARTESIAN_POINT ( 'NONE',  ( -144.8060344827586050, -7.497491405672223941, -2.775557561562891351E-14 ) ) ;
#384 = CARTESIAN_POINT ( 'NONE',  ( -281.4538215477170979, 269.4574776399289249, -145.6842353883612304 ) ) ;
#385 = CARTESIAN_POINT ( 'NONE',  ( 24.83884780301425721, -996.7275481119215783, 145.0000119999999981 ) ) ;
#386 = LINE ( 'NONE', #9552, #2401 ) ;
#387 = LINE ( 'NONE', #18240, #3022 ) ;
#388 = ORIENTED_EDGE ( 'NONE', *, *, #7363, .F. ) ;
#389 = DIRECTION ( 'NONE',  ( 0.000000000000000000, 0.000000000000000000, -1.000000000000000000 ) ) ;
#390 = CARTESIAN_POINT ( 'NONE',  ( -2.621328321948020346, -7.606199919102354379, -7.633618187056584681 ) ) ;
#392 = ORIENTED_EDGE ( 'NONE', *, *, #11920, .F. ) ;
#391 = ORIENTED_EDGE ( 'NONE', *, *, #9476, .F. ) ;
#394 = AXIS2_PLACEMENT_3D ( 'NONE', #13322, #2647, #11500 ) ;
#393 = AXIS2_PLACEMENT_3D ( 'NONE', #13727, #20924, #11913 ) ;
#395 = CARTESIAN_POINT ( 'NONE',  ( 51.87806360044629628, 135.4018704341563364, -90.00000000000000000 ) ) ;
#396 = CARTESIAN_POINT ( 'NONE',  ( 280.4976310729377929, 272.3436892194421830, -147.6188186979286456 ) ) ;
#397 = VECTOR ( 'NONE', #5693, 1000.000000000000000 ) ;
#398 = AXIS2_PLACEMENT_3D ( 'NONE', #21012, #4473, #22453 ) ;
#399 = CIRCLE ( 'NONE', #7721, 7.499999999999996447 ) ;
#400 = ORIENTED_EDGE ( 'NONE', *, *, #3148, .F. ) ;
#401 = CARTESIAN_POINT ( 'NONE',  ( -135.6291186032800340, -1075.032345129804526, 27.50000000000644462 ) ) ;
#402 = EDGE_LOOP ( 'NONE', ( #16572, #22684, #22058, #9340 ) ) ;
#403 = DIRECTION ( 'NONE',  ( -1.000000000000000000, -0.000000000000000000, -0.000000000000000000 ) ) ;
#404 = VERTEX_POINT ( 'NONE', #6272 ) ;
#405 = CARTESIAN_POINT ( 'NONE',  ( 0.2500000000000002220, 0.000000000000000000, 0.000000000000000000 ) ) ;
#406 = LINE ( 'NONE', #11777, #11576 ) ;
#407 = ITEM_DEFINED_TRANSFORMATION ( 'NONE', 'NONE', #14309,  #11210 ) ;
#408 = EDGE_LOOP ( 'NONE', ( #13724, #11220, #22604, #14081, #3269 ) ) ;
#409 = CARTESIAN_POINT ( 'NONE',  ( 2.500000000000000000, -2.357898499370432610, 3.252606517456513302E-15 ) ) ;
#410 = AXIS2_PLACEMENT_3D ( 'NONE', #20070, #5692, #13105 ) ;
#411 = ORIENTED_EDGE ( 'NONE', *, *, #12338, .T. ) ;
#412 = CARTESIAN_POINT ( 'NONE',  ( -128.8385278530645905, 86.17219694792730422, 28.11255663403418126 ) ) ;
#413 = AXIS2_PLACEMENT_3D ( 'NONE', #9639, #22415, #8058 ) ;
#414 =( LENGTH_UNIT ( ) NAMED_UNIT ( * ) SI_UNIT ( .MILLI., .METRE. ) );
#415 = EDGE_CURVE ( 'NONE', #12774, #3203, #17606, .T. ) ;
#416 = CIRCLE ( 'NONE', #20853, 2.649999999999975486 ) ;
#417 = AXIS2_PLACEMENT_3D ( 'NONE', #10094, #19108, #10454 ) ;
#418 = DIRECTION ( 'NONE',  ( 1.000000000000000000, 3.202566417187951028E-16, 6.405132834375902056E-16 ) ) ;
#419 = DIRECTION ( 'NONE',  ( 0.000000000000000000, 1.177509268541832635E-16, -1.000000000000000000 ) ) ;
#420 = ORIENTED_EDGE ( 'NONE', *, *, #2725, .F. ) ;
#421 = CARTESIAN_POINT ( 'NONE',  ( -280.1244266708878854, 270.0000000000000000, -145.2880230824753198 ) ) ;
#422 = VERTEX_POINT ( 'NONE', #11864 ) ;
#423 = EDGE_CURVE ( 'NONE', #23301, #11044, #12932, .T. ) ;
#424 = DIRECTION ( 'NONE',  ( 0.000000000000000000, 0.000000000000000000, 1.000000000000000000 ) ) ;
#425 = CARTESIAN_POINT ( 'NONE',  ( -7.808218555863076560, -4.508077085118260108, -7.999534413642739317 ) ) ;
#426 = CARTESIAN_POINT ( 'NONE',  ( 132.5032837044622056, 80.42329363488276783, -27.57873596473011446 ) ) ;
#427 = ADVANCED_FACE ( 'NONE', ( #15825 ), #831, .F. ) ;
#428 = DIRECTION ( 'NONE',  ( 0.000000000000000000, 1.000000000000000000, -3.502807018799300809E-15 ) ) ;
#429 = DIRECTION ( 'NONE',  ( 1.000000000000000000, 0.000000000000000000, 0.000000000000000000 ) ) ;
#430 = EDGE_LOOP ( 'NONE', ( #19662, #7339, #6676, #22145 ) ) ;
#431 = EDGE_CURVE ( 'NONE', #23382, #2113, #16801, .T. ) ;
#432 = CARTESIAN_POINT ( 'NONE',  ( -8.354408924214205001, 5.621797280079010584, 200.0000120000000550 ) ) ;
#433 = CARTESIAN_POINT ( 'NONE',  ( 0.000000000000000000, 1.178949249685213863, -2.042000000000001148 ) ) ;
#434 = LINE ( 'NONE', #15168, #15820 ) ;
#435 = CONTEXT_DEPENDENT_SHAPE_REPRESENTATION ( #15110, #15870 ) ;
#436 = VERTEX_POINT ( 'NONE', #17740 ) ;
#437 = LINE ( 'NONE', #21907, #19401 ) ;
#438 = EDGE_LOOP ( 'NONE', ( #2564, #18535, #16331, #17090, #23545 ) ) ;
#439 = DIRECTION ( 'NONE',  ( 1.000000000000000000, -0.000000000000000000, 6.982962677686266711E-15 ) ) ;
#440 = DIRECTION ( 'NONE',  ( 1.000000000000000000, 0.000000000000000000, 0.000000000000000000 ) ) ;
#441 = FACE_OUTER_BOUND ( 'NONE', #10647, .T. ) ;
#442 = VERTEX_POINT ( 'NONE', #8210 ) ;
#443 = DIRECTION ( 'NONE',  ( -1.000000000000000000, 0.000000000000000000, 0.000000000000000000 ) ) ;
#444 = FACE_BOUND ( 'NONE', #1590, .T. ) ;
#445 = DIRECTION ( 'NONE',  ( -0.000000000000000000, -0.000000000000000000, 1.000000000000000000 ) ) ;
#446 = DIRECTION ( 'NONE',  ( 0.000000000000000000, -1.177509268541832635E-16, 1.000000000000000000 ) ) ;
#447 = DIRECTION ( 'NONE',  ( 0.000000000000000000, 0.000000000000000000, 1.000000000000000000 ) ) ;
#448 = CARTESIAN_POINT ( 'NONE',  ( 70.00000000000000000, -87.33333333333332860, 124.9999999999999858 ) ) ;
#449 = LINE ( 'NONE', #9746, #13276 ) ;
#450 = ORIENTED_EDGE ( 'NONE', *, *, #16095, .T. ) ;
#451 = FILL_AREA_STYLE ('',( #1678 ) ) ;
#452 = CARTESIAN_POINT ( 'NONE',  ( 0.000000000000000000, 0.000000000000000000, 90.00000000000000000 ) ) ;
#453 = DIRECTION ( 'NONE',  ( 0.000000000000000000, 0.000000000000000000, 1.000000000000000000 ) ) ;
#454 = ORIENTED_EDGE ( 'NONE', *, *, #4695, .F. ) ;
#455 = ORIENTED_EDGE ( 'NONE', *, *, #19160, .F. ) ;
#456 = PLANE ( 'NONE',  #413 ) ;
#457 = CARTESIAN_POINT ( 'NONE',  ( 153.5653415408403646, -1122.352966361445169, 30.00000000000675726 ) ) ;
#458 = ADVANCED_FACE ( 'NONE', ( #6629 ), #8833, .F. ) ;
#459 = CARTESIAN_POINT ( 'NONE',  ( 282.1854425596106921, 268.0906609804447953, -146.3673129565597719 ) ) ;
#460 = EDGE_CURVE ( 'NONE', #4025, #10987, #14591, .T. ) ;
#461 = EDGE_LOOP ( 'NONE', ( #908, #4370, #8639, #3777 ) ) ;
#462 = DIRECTION ( 'NONE',  ( -0.7232617928448825673, 0.6905739489807055653, 6.982962677686266711E-15 ) ) ;
#463 = ADVANCED_FACE ( 'NONE', ( #11105 ), #20128, .F. ) ;
#464 = DIRECTION ( 'NONE',  ( 1.000000000000000000, 0.000000000000000000, 0.000000000000000000 ) ) ;
#465 = ORIENTED_EDGE ( 'NONE', *, *, #13801, .F. ) ;
#466 = DIRECTION ( 'NONE',  ( 0.000000000000000000, 0.000000000000000000, 1.000000000000000000 ) ) ;
#467 = DIRECTION ( 'NONE',  ( 0.9510565162951580831, -0.3090169943749334069, 0.000000000000000000 ) ) ;
#468 = ADVANCED_FACE ( 'NONE', ( #22056 ), #1764, .F. ) ;
#469 = UNCERTAINTY_MEASURE_WITH_UNIT (LENGTH_MEASURE( 1.000000000000000082E-05 ), #4859, 'distance_accuracy_value', 'NONE');
#470 = CARTESIAN_POINT ( 'NONE',  ( 0.000000000000000000, 4.685197434473814759, -5.637851296924623057E-15 ) ) ;
#471 = VERTEX_POINT ( 'NONE', #10993 ) ;
#472 = CARTESIAN_POINT ( 'NONE',  ( 281.9223300543793584, 268.9079617568158938, -145.9952621458755857 ) ) ;
#473 = ITEM_DEFINED_TRANSFORMATION ( 'NONE', 'NONE', #7714,  #11210 ) ;
#474 = FACE_OUTER_BOUND ( 'NONE', #7021, .T. ) ;
#475 = CARTESIAN_POINT ( 'NONE',  ( -64.99999999999995737, -56.79999999999964899, 65.00000000000018474 ) ) ;
#476 = DIRECTION ( 'NONE',  ( -0.000000000000000000, -0.000000000000000000, 1.000000000000000000 ) ) ;
#477 = ORIENTED_EDGE ( 'NONE', *, *, #2966, .T. ) ;
#478 = ORIENTED_EDGE ( 'NONE', *, *, #11288, .T. ) ;
#479 = CARTESIAN_POINT ( 'NONE',  ( -3.000000000000002665, 0.000000000000000000, 0.000000000000000000 ) ) ;
#480 = CARTESIAN_POINT ( 'NONE',  ( -146.4450000000005332, -784.4690652294799520, -29.99999999999356248 ) ) ;
#481 = ADVANCED_FACE ( 'NONE', ( #3691 ), #14484, .T. ) ;
#482 = CARTESIAN_POINT ( 'NONE',  ( -6.902527771671634227, -4.675077770780906583, -0.7026937717022867513 ) ) ;
#483 = CARTESIAN_POINT ( 'NONE',  ( -127.9021285790841205, 87.55595642181887683, 27.50000000000646239 ) ) ;
#484 = EDGE_LOOP ( 'NONE', ( #635, #3339, #8583, #20621 ) ) ;
#485 = CARTESIAN_POINT ( 'NONE',  ( -45.00000000000000000, 272.9999999999999432, 0.000000000000000000 ) ) ;
#486 = VECTOR ( 'NONE', #22174, 1000.000000000000000 ) ;
#487 = ORIENTED_EDGE ( 'NONE', *, *, #3373, .T. ) ;
#488 = EDGE_CURVE ( 'NONE', #4511, #21370, #19433, .T. ) ;
#489 = DIRECTION ( 'NONE',  ( -1.000000000000000000, -0.000000000000000000, -0.000000000000000000 ) ) ;
#490 = EDGE_CURVE ( 'NONE', #8328, #14713, #20594, .T. ) ;
#491 = DIRECTION ( 'NONE',  ( 0.000000000000000000, 0.000000000000000000, -1.000000000000000000 ) ) ;
#492 = ORIENTED_EDGE ( 'NONE', *, *, #8852, .T. ) ;
#493 = VERTEX_POINT ( 'NONE', #1420 ) ;
#494 = CARTESIAN_POINT ( 'NONE',  ( 2.500000000000000000, 2.357898499370431722, -2.818925648462311528E-15 ) ) ;
#495 = FACE_OUTER_BOUND ( 'NONE', #9438, .T. ) ;
#496 = CARTESIAN_POINT ( 'NONE',  ( -24.99999999999998224, -1000.000000000000000, -145.0000060000000417 ) ) ;
#497 = CARTESIAN_POINT ( 'NONE',  ( -280.1452901038203436, 270.0000000000000000, -145.0627656775836556 ) ) ;
#498 = DIRECTION ( 'NONE',  ( -0.000000000000000000, 0.000000000000000000, -1.000000000000000000 ) ) ;
#499 = DIRECTION ( 'NONE',  ( 0.000000000000000000, 0.000000000000000000, 1.000000000000000000 ) ) ;
#500 = DIRECTION ( 'NONE',  ( 0.000000000000000000, -3.495664435217746987E-15, -1.000000000000000000 ) ) ;
#501 = EDGE_LOOP ( 'NONE', ( #8871, #21661, #12574, #4452 ) ) ;
#502 = FACE_BOUND ( 'NONE', #1152, .T. ) ;
#503 = DIRECTION ( 'NONE',  ( 0.000000000000000000, 0.000000000000000000, 1.000000000000000000 ) ) ;
#504 = CONTEXT_DEPENDENT_SHAPE_REPRESENTATION ( #11411, #10489 ) ;
#505 = VECTOR ( 'NONE', #4591, 1000.000000000000000 ) ;
#506 = VERTEX_POINT ( 'NONE', #7097 ) ;
#507 = CARTESIAN_POINT ( 'NONE',  ( -136.9304241666588666, -1072.629629052829387, -29.19154146838981490 ) ) ;
#508 = CARTESIAN_POINT ( 'NONE',  ( -90.00000000000000000, -76.73205080756885366, 3.000000000000002665 ) ) ;
#509 = ORIENTED_EDGE ( 'NONE', *, *, #16797, .F. ) ;
#510 = ADVANCED_FACE ( 'NONE', ( #8805 ), #10215, .F. ) ;
#511 = FACE_OUTER_BOUND ( 'NONE', #7299, .T. ) ;
#512 = ORIENTED_EDGE ( 'NONE', *, *, #2203, .T. ) ;
#513 = DIRECTION ( 'NONE',  ( -0.7071067811865320296, 9.875400524328840493E-15, 0.7071067811865631159 ) ) ;
#514 = ORIENTED_EDGE ( 'NONE', *, *, #11865, .F. ) ;
#515 = EDGE_CURVE ( 'NONE', #17412, #8986, #3345, .T. ) ;
#516 = DIRECTION ( 'NONE',  ( -1.000000000000000000, -0.000000000000000000, -0.000000000000000000 ) ) ;
#517 = DIRECTION ( 'NONE',  ( -0.000000000000000000, -0.000000000000000000, 1.000000000000000000 ) ) ;
#518 = CONTEXT_DEPENDENT_SHAPE_REPRESENTATION ( #9897, #11475 ) ;
#519 = ORIENTED_EDGE ( 'NONE', *, *, #14734, .F. ) ;
#520 =( BOUNDED_SURFACE ( )  B_SPLINE_SURFACE ( 3, 2, ( 
 ( #8768, #10596, #14345 ),
 ( #16129, #20203, #12794 ),
 ( #5133, #12544, #19859 ),
 ( #3307, #8898, #16259 ),
 ( #23601, #7057, #14447 ),
 ( #7298, #3652, #21785 ) ),
 .UNSPECIFIED., .F., .F., .F. ) 
 B_SPLINE_SURFACE_WITH_KNOTS ( ( 4, 2, 4 ),
 ( 3, 3 ),
 ( 0.02032853247518125531, 0.02278863295364820865, 0.02524873343211516200 ),
 ( 0.000000000000000000, 1.000000000000000000 ),
 .UNSPECIFIED. ) 
 GEOMETRIC_REPRESENTATION_ITEM ( )  RATIONAL_B_SPLINE_SURFACE ( (
 ( 1.000000000000000000, 0.8047781615896836271, 1.000000000000000000),
 ( 1.000000000000000000, 0.8123767586289967202, 1.000000000000000000),
 ( 1.000000000000000000, 0.8190662415563443322, 1.000000000000000000),
 ( 1.000000000000000000, 0.8192361015669982205, 1.000000000000000000),
 ( 1.000000000000000000, 0.8126135807103181952, 1.000000000000000000),
 ( 1.000000000000000000, 0.8047712338318587788, 1.000000000000000000) ) ) 
 REPRESENTATION_ITEM ( '' )  SURFACE ( )  );
#521 = AXIS2_PLACEMENT_3D ( 'NONE', #1409, #23626, #7438 ) ;
#522 = EDGE_CURVE ( 'NONE', #18839, #1157, #6119, .T. ) ;
#523 = DIRECTION ( 'NONE',  ( -1.000000000000000000, -2.775557561562891351E-17, -0.000000000000000000 ) ) ;
#524 = EDGE_LOOP ( 'NONE', ( #4189, #16667, #22630, #21113 ) ) ;
#525 = CARTESIAN_POINT ( 'NONE',  ( 5.200000000000020606, 0.000000000000000000, 2.499999999999993339 ) ) ;
#526 = CARTESIAN_POINT ( 'NONE',  ( -3.511755186886750479, 2.826662030176366081, -3.597382984111578086 ) ) ;
#527 = LINE ( 'NONE', #18858, #1845 ) ;
#528 = CARTESIAN_POINT ( 'NONE',  ( -90.00000000000000000, 75.00000000000001421, 0.000000000000000000 ) ) ;
#529 = ORIENTED_EDGE ( 'NONE', *, *, #11440, .F. ) ;
#530 = CARTESIAN_POINT ( 'NONE',  ( -282.0873946496627127, 268.5095819834011763, 146.1815513148989965 ) ) ;
#531 = AXIS2_PLACEMENT_3D ( 'NONE', #16784, #7738, #20398 ) ;
#533 = ORIENTED_EDGE ( 'NONE', *, *, #2318, .F. ) ;
#532 = ORIENTED_EDGE ( 'NONE', *, *, #21218, .F. ) ;
#534 = CARTESIAN_POINT ( 'NONE',  ( 131.4546237677520253, -1099.567474056936362, 30.00000000000653699 ) ) ;
#535 = PLANE ( 'NONE',  #3468 ) ;
#536 = FACE_OUTER_BOUND ( 'NONE', #16343, .T. ) ;
#537 = CARTESIAN_POINT ( 'NONE',  ( -79.99999999999997158, -62.00000000000001421, 5.199999999999997513 ) ) ;
#538 = CARTESIAN_POINT ( 'NONE',  ( 0.000000000000000000, 0.000000000000000000, -9.974600000000000577 ) ) ;
#539 = VERTEX_POINT ( 'NONE', #2242 ) ;
#540 = CARTESIAN_POINT ( 'NONE',  ( 2.500000000000000000, 2.357898499370433054, -1.951563910473907981E-15 ) ) ;
#541 = CYLINDRICAL_SURFACE ( 'NONE', #20678, 2.199999999999979750 ) ;
#542 = CARTESIAN_POINT ( 'NONE',  ( 102.3500000000000227, 35.00000000000000000, 0.000000000000000000 ) ) ;
#543 = EDGE_LOOP ( 'NONE', ( #6408, #4802, #11435, #2542 ) ) ;
#544 = ADVANCED_FACE ( 'NONE', ( #5876 ), #11344, .F. ) ;
#546 = CYLINDRICAL_SURFACE ( 'NONE', #5912, 20.00000000000000000 ) ;
#545=STYLED_ITEM('',(#23920),#12018);
#547 = ORIENTED_EDGE ( 'NONE', *, *, #19326, .F. ) ;
#548 = DIRECTION ( 'NONE',  ( -3.700743415417187942E-15, 1.000000000000000000, 0.000000000000000000 ) ) ;
#549 = CARTESIAN_POINT ( 'NONE',  ( -280.0000000000000568, 272.9999999999999432, 145.0000000000000284 ) ) ;
#550 = VERTEX_POINT ( 'NONE', #7568 ) ;
#551 = CARTESIAN_POINT ( 'NONE',  ( 7.500000000000000000, 4.330127018922199866, -1.000000000000000888 ) ) ;
#552 = ORIENTED_EDGE ( 'NONE', *, *, #1635, .T. ) ;
#553 = CARTESIAN_POINT ( 'NONE',  ( 0.000000000000000000, 2.357898499370434386, -3.469446951953614189E-15 ) ) ;
#554 = CARTESIAN_POINT ( 'NONE',  ( 0.000000000000000000, 0.000000000000000000, -90.00000000000000000 ) ) ;
#555 = CARTESIAN_POINT ( 'NONE',  ( -69.99999999999997158, -112.6666666666667140, 3.000000000000000000 ) ) ;
#556 = CARTESIAN_POINT ( 'NONE',  ( 3.679171394226031122, 2.494631558665830973, -0.3503314178412474389 ) ) ;
#557 = FACE_OUTER_BOUND ( 'NONE', #1366, .T. ) ;
#558 = EDGE_CURVE ( 'NONE', #7386, #12822, #19852, .T. ) ;
#559 = CARTESIAN_POINT ( 'NONE',  ( -288.2000000000013529, -89.99999999999897682, 26.98333333333330231 ) ) ;
#560 = DIRECTION ( 'NONE',  ( 0.000000000000000000, 0.000000000000000000, -1.000000000000000000 ) ) ;
#561 = ORIENTED_EDGE ( 'NONE', *, *, #3975, .T. ) ;
#562 = FACE_BOUND ( 'NONE', #6176, .T. ) ;
#563 = DIRECTION ( 'NONE',  ( 0.000000000000000000, 0.000000000000000000, 1.000000000000000000 ) ) ;
#564 = ORIENTED_EDGE ( 'NONE', *, *, #13021, .F. ) ;
#565 = EDGE_LOOP ( 'NONE', ( #2782, #21644, #4251, #22366 ) ) ;
#566 = VECTOR ( 'NONE', #11218, 1000.000000000000000 ) ;
#567 = FACE_OUTER_BOUND ( 'NONE', #20459, .T. ) ;
#569 = AXIS2_PLACEMENT_3D ( 'NONE', #10338, #15656, #17679 ) ;
#568 = DIRECTION ( 'NONE',  ( -1.000000000000000000, -0.000000000000000000, -0.000000000000000000 ) ) ;
#570 = FACE_OUTER_BOUND ( 'NONE', #6214, .T. ) ;
#571 = CIRCLE ( 'NONE', #7503, 2.649999999999971934 ) ;
#572 = ORIENTED_EDGE ( 'NONE', *, *, #16103, .T. ) ;
#573 = FACE_OUTER_BOUND ( 'NONE', #17478, .T. ) ;
#574 = CARTESIAN_POINT ( 'NONE',  ( -69.99999999999997158, -112.6666666666667140, 124.9999999999999858 ) ) ;
#575 = DIRECTION ( 'NONE',  ( 0.000000000000000000, 1.000000000000000000, 0.000000000000000000 ) ) ;
#576 = ORIENTED_EDGE ( 'NONE', *, *, #2075, .T. ) ;
#577 = EDGE_CURVE ( 'NONE', #539, #10685, #15195, .T. ) ;
#578 = FACE_OUTER_BOUND ( 'NONE', #18911, .T. ) ;
#579 = CARTESIAN_POINT ( 'NONE',  ( 2.500000000000000000, -1.178949249685218081, -2.041999999999998039 ) ) ;
#580 = EDGE_CURVE ( 'NONE', #1699, #1893, #14858, .T. ) ;
#581 = SURFACE_SIDE_STYLE ('',( #17124 ) ) ;
#582 = ORIENTED_EDGE ( 'NONE', *, *, #10189, .T. ) ;
#583 = DIRECTION ( 'NONE',  ( -0.000000000000000000, 0.000000000000000000, 1.000000000000000000 ) ) ;
#584 = FACE_BOUND ( 'NONE', #11064, .T. ) ;
#585 = EDGE_CURVE ( 'NONE', #16285, #2501, #3259, .T. ) ;
#586 = CARTESIAN_POINT ( 'NONE',  ( -146.0000000000005684, -496.5240652294801293, -29.99999999999356604 ) ) ;
#587 = DIRECTION ( 'NONE',  ( -6.676953772165163028E-17, -0.8660254037844398178, -0.4999999999999980571 ) ) ;
#588 =( GEOMETRIC_REPRESENTATION_CONTEXT ( 3 ) GLOBAL_UNCERTAINTY_ASSIGNED_CONTEXT ( ( #4447 ) ) GLOBAL_UNIT_ASSIGNED_CONTEXT ( ( #9575, #6058, #2789 ) ) REPRESENTATION_CONTEXT ( 'NONE', 'WORKASPACE' ) );
#589 = CLOSED_SHELL ( 'NONE', ( #11368, #788, #23385, #20795, #2609, #21444, #6790, #9900, #8687, #7105, #11204, #10218, #16290, #19058, #463, #16239, #358, #10479, #18110, #9024, #1914, #5319, #16488, #1601, #20906, #2345, #19700, #11952, #5464, #626, #8870, #13898, #20498, #5716, #16281, #4561, #17901, #4387, #5710, #23652, #11628, #12501, #17871, #17586, #23607, #23039, #14935, #17741, #20750, #1436 ) ) ;
#590 = VERTEX_POINT ( 'NONE', #22650 ) ;
#591 = ORIENTED_EDGE ( 'NONE', *, *, #17311, .T. ) ;
#592 = DIRECTION ( 'NONE',  ( -2.775557561562891351E-17, 1.000000000000000000, -1.850371707708594366E-15 ) ) ;
#593 = CARTESIAN_POINT ( 'NONE',  ( 2.500000000000000000, 2.357898499370432166, -2.385244779468109755E-15 ) ) ;
#594 = EDGE_CURVE ( 'NONE', #15324, #17025, #2363, .T. ) ;
#595 = VECTOR ( 'NONE', #12133, 1000.000000000000000 ) ;
#596 =( REPRESENTATION_RELATIONSHIP ('NONE','NONE', #10127, #18083 ) REPRESENTATION_RELATIONSHIP_WITH_TRANSFORMATION ( #10136 )SHAPE_REPRESENTATION_RELATIONSHIP( ) );
#597 = DIRECTION ( 'NONE',  ( 1.000000000000000000, -0.000000000000000000, 6.982962677686266711E-15 ) ) ;
#598 = CARTESIAN_POINT ( 'NONE',  ( -126.4561707720357191, 89.63167338449062527, 29.67072815018523357 ) ) ;
#599 = ORIENTED_EDGE ( 'NONE', *, *, #1215, .T. ) ;
#600 = CARTESIAN_POINT ( 'NONE',  ( 2.100000000000000089, 0.000000000000000000, -4.694516984716113228 ) ) ;
#601 = VECTOR ( 'NONE', #6636, 1000.000000000000000 ) ;
#602 = CIRCLE ( 'NONE', #4405, 0.7733184030943203169 ) ;
#603 = VERTEX_POINT ( 'NONE', #15316 ) ;
#604 = CARTESIAN_POINT ( 'NONE',  ( 285.2000000000008981, 9.892604858775018348E-13, 146.4928932188134638 ) ) ;
#605 = CARTESIAN_POINT ( 'NONE',  ( 158.0000000000000284, -500.0000000000000000, 32.64999999999999858 ) ) ;
#606 = ORIENTED_EDGE ( 'NONE', *, *, #5631, .F. ) ;
#607 = EDGE_LOOP ( 'NONE', ( #10309, #6609 ) ) ;
#608 = FACE_OUTER_BOUND ( 'NONE', #10956, .T. ) ;
#609 = PRODUCT_DEFINITION_SHAPE ( 'NONE', 'NONE',  #23855 ) ;
#610 = DIRECTION ( 'NONE',  ( -1.000000000000000000, -2.775557561562891351E-17, -0.000000000000000000 ) ) ;
#611 = CIRCLE ( 'NONE', #234, 2.100000000000000089 ) ;
#612 = CARTESIAN_POINT ( 'NONE',  ( -3.267023609986814847, -1024.839877336693462, -145.0000000000001421 ) ) ;
#613 = EDGE_CURVE ( 'NONE', #10116, #16453, #2122, .T. ) ;
#614 = CARTESIAN_POINT ( 'NONE',  ( 280.6822561791009889, 272.9663407402829876, 145.1247002395580807 ) ) ;
#615 = CARTESIAN_POINT ( 'NONE',  ( 18.83467029480909005, -983.4793312354817090, 145.0000119999999697 ) ) ;
#616 = ADVANCED_FACE ( 'NONE', ( #7814 ), #9512, .F. ) ;
#617 = CARTESIAN_POINT ( 'NONE',  ( 40.00000000000000000, 100.0000000000000000, 150.2000000000009550 ) ) ;
#618 = ORIENTED_EDGE ( 'NONE', *, *, #2883, .F. ) ;
#619 = EDGE_CURVE ( 'NONE', #20328, #13113, #6356, .T. ) ;
#620 = CARTESIAN_POINT ( 'NONE',  ( -5.335963852939856089, -6.035591050534137025, -7.593821156097342318 ) ) ;
#621 = SURFACE_SIDE_STYLE ('',( #11763 ) ) ;
#622 = EDGE_LOOP ( 'NONE', ( #22663, #20160, #16621, #5819 ) ) ;
#623 = EDGE_CURVE ( 'NONE', #21238, #949, #17113, .T. ) ;
#624 = CARTESIAN_POINT ( 'NONE',  ( -136.9597779064870053, -1072.574344195403910, -30.66034227022094072 ) ) ;
#625 = DIRECTION ( 'NONE',  ( -0.000000000000000000, -0.000000000000000000, 1.000000000000000000 ) ) ;
#626 = ADVANCED_FACE ( 'NONE', ( #13405, #570 ), #13541, .T. ) ;
#627 = ORIENTED_EDGE ( 'NONE', *, *, #7371, .F. ) ;
#628 = DIRECTION ( 'NONE',  ( 1.000000000000000000, 0.000000000000000000, 0.000000000000000000 ) ) ;
#629 = VERTEX_POINT ( 'NONE', #2837 ) ;
#630 = CARTESIAN_POINT ( 'NONE',  ( 57.99999999999997868, -62.00000000000001421, -3.122502256758252770E-14 ) ) ;
#631 = CARTESIAN_POINT ( 'NONE',  ( 282.6045710003933777, 272.3135885331259942, -145.4973317504631609 ) ) ;
#632 = EDGE_LOOP ( 'NONE', ( #21838, #2466, #15904, #21981 ) ) ;
#633 = DIRECTION ( 'NONE',  ( -0.000000000000000000, -0.000000000000000000, 1.000000000000000000 ) ) ;
#634 = DIRECTION ( 'NONE',  ( -1.000000000000000000, 1.408839003528726857E-14, 6.982962677686266711E-15 ) ) ;
#635 = ORIENTED_EDGE ( 'NONE', *, *, #22905, .T. ) ;
#636 = DIRECTION ( 'NONE',  ( 1.000000000000000000, 0.000000000000000000, 0.000000000000000000 ) ) ;
#637 = DIRECTION ( 'NONE',  ( -0.000000000000000000, -0.000000000000000000, 1.000000000000000000 ) ) ;
#638 = CARTESIAN_POINT ( 'NONE',  ( 158.0000000000000284, -490.0000000000001137, -56.99999999999996447 ) ) ;
#639 = LINE ( 'NONE', #8009, #11174 ) ;
#640 = VERTEX_POINT ( 'NONE', #19144 ) ;
#641 = CARTESIAN_POINT ( 'NONE',  ( -281.3684665762324926, 268.0840560642351988, -147.1696999999999207 ) ) ;
#642 = AXIS2_PLACEMENT_3D ( 'NONE', #1473, #5465, #8869 ) ;
#643 = AXIS2_PLACEMENT_3D ( 'NONE', #14419, #1236, #23084 ) ;
#645 = ORIENTED_EDGE ( 'NONE', *, *, #15881, .F. ) ;
#644 = VERTEX_POINT ( 'NONE', #21439 ) ;
#646 = DIRECTION ( 'NONE',  ( 0.7232617928448825673, -0.6905739489807055653, -6.982962677686266711E-15 ) ) ;
#647 = EDGE_CURVE ( 'NONE', #8521, #1528, #10238, .T. ) ;
#648 = CARTESIAN_POINT ( 'NONE',  ( 155.0000000000000568, -801.0618695410399823, 32.50000000000648015 ) ) ;
#649 = CYLINDRICAL_SURFACE ( 'NONE', #1566, 160.0000000000000000 ) ;
#650 = EDGE_CURVE ( 'NONE', #19885, #23227, #1024, .T. ) ;
#651 = CARTESIAN_POINT ( 'NONE',  ( 235.0000000000000284, 6.522560269672795464E-15, 0.000000000000000000 ) ) ;
#652 = FACE_OUTER_BOUND ( 'NONE', #16462, .T. ) ;
#653 = ORIENTED_EDGE ( 'NONE', *, *, #14771, .F. ) ;
#654 = DIRECTION ( 'NONE',  ( 1.000000000000000000, 0.000000000000000000, 0.000000000000000000 ) ) ;
#655 = CIRCLE ( 'NONE', #14181, 2.649999999999971934 ) ;
#656 = DIRECTION ( 'NONE',  ( 1.350636282998972974E-14, 0.000000000000000000, -1.000000000000000000 ) ) ;
#657 = DIRECTION ( 'NONE',  ( 0.000000000000000000, 1.177509268541832635E-16, -1.000000000000000000 ) ) ;
#658 = ORIENTED_EDGE ( 'NONE', *, *, #12364, .F. ) ;
#659 = DIRECTION ( 'NONE',  ( 1.000000000000000000, 0.000000000000000000, 0.000000000000000000 ) ) ;
#660 = ORIENTED_EDGE ( 'NONE', *, *, #11816, .T. ) ;
#661 = CARTESIAN_POINT ( 'NONE',  ( -90.00000000000000000, -79.73205080756885366, 3.000000000000002665 ) ) ;
#662 = CARTESIAN_POINT ( 'NONE',  ( -285.2000000000013529, -89.99999999999896261, -40.33333333333332860 ) ) ;
#663 = ORIENTED_EDGE ( 'NONE', *, *, #16433, .T. ) ;
#664 = CARTESIAN_POINT ( 'NONE',  ( 3.000000000000002665, 0.000000000000000000, 0.000000000000000000 ) ) ;
#665 = ORIENTED_EDGE ( 'NONE', *, *, #13392, .T. ) ;
#666 = DIRECTION ( 'NONE',  ( -0.000000000000000000, -0.000000000000000000, 1.000000000000000000 ) ) ;
#667 = VECTOR ( 'NONE', #14846, 1000.000000000000114 ) ;
#668 = FACE_BOUND ( 'NONE', #1708, .T. ) ;
#669 = CARTESIAN_POINT ( 'NONE',  ( 0.000000000000000000, 0.000000000000000000, -90.00000000000000000 ) ) ;
#670 = LINE ( 'NONE', #6231, #14453 ) ;
#671 = CARTESIAN_POINT ( 'NONE',  ( 2.700000000000001066, 3.061616997868383043E-15, 25.00000000000000000 ) ) ;
#672 = PLANE ( 'NONE',  #1139 ) ;
#673 = CARTESIAN_POINT ( 'NONE',  ( -7.894706624614703294, -0.7534108004380160040, -7.590222617908770175 ) ) ;
#674 = ORIENTED_EDGE ( 'NONE', *, *, #10081, .T. ) ;
#675 = FACE_BOUND ( 'NONE', #20400, .T. ) ;
#676 = VECTOR ( 'NONE', #16342, 1000.000000000000000 ) ;
#677 = DIRECTION ( 'NONE',  ( 1.350636282998972974E-14, 0.000000000000000000, -1.000000000000000000 ) ) ;
#678 = AXIS2_PLACEMENT_3D ( 'NONE', #5455, #7253, #20169 ) ;
#679 = VERTEX_POINT ( 'NONE', #17578 ) ;
#680 = ORIENTED_EDGE ( 'NONE', *, *, #10475, .T. ) ;
#681 = CARTESIAN_POINT ( 'NONE',  ( 2.670021022440450587, 9.709363531332249053, 200.0000120000000265 ) ) ;
#682 = CARTESIAN_POINT ( 'NONE',  ( 0.000000000000000000, 1.178949249685218525, 2.041999999999999371 ) ) ;
#683 = DIRECTION ( 'NONE',  ( 0.000000000000000000, 1.103561164596346103E-15, 1.000000000000000000 ) ) ;
#684 = ORIENTED_EDGE ( 'NONE', *, *, #8782, .F. ) ;
#685 = CARTESIAN_POINT ( 'NONE',  ( 0.000000000000000000, 0.000000000000000000, 0.000000000000000000 ) ) ;
#686 = DIRECTION ( 'NONE',  ( -1.000000000000000000, 3.495664435217746592E-15, -0.000000000000000000 ) ) ;
#687 = DIRECTION ( 'NONE',  ( -1.000000000000000000, -0.000000000000000000, -0.000000000000000000 ) ) ;
#688 = ORIENTED_EDGE ( 'NONE', *, *, #3854, .T. ) ;
#689 = FACE_OUTER_BOUND ( 'NONE', #8839, .T. ) ;
#690 = CIRCLE ( 'NONE', #14219, 5.000000000000000888 ) ;
#691 = DIRECTION ( 'NONE',  ( 0.000000000000000000, -1.177509268541832635E-16, 1.000000000000000000 ) ) ;
#692 = VECTOR ( 'NONE', #7161, 1000.000000000000000 ) ;
#693 = ORIENTED_EDGE ( 'NONE', *, *, #16007, .T. ) ;
#694 = DIRECTION ( 'NONE',  ( 1.000000000000000000, 3.469446951953617640E-16, 8.673617379884035472E-17 ) ) ;
#695 = AXIS2_PLACEMENT_3D ( 'NONE', #11043, #18024, #7144 ) ;
#696 = DIRECTION ( 'NONE',  ( 1.000000000000000000, 0.000000000000000000, 0.000000000000000000 ) ) ;
#697 = CARTESIAN_POINT ( 'NONE',  ( -282.2000000000006708, 90.00000000000102318, -32.35000000000004405 ) ) ;
#698 = CARTESIAN_POINT ( 'NONE',  ( -31.74999999999995737, 0.000000000000000000, 2.500000000000000444 ) ) ;
#699 = ORIENTED_EDGE ( 'NONE', *, *, #6704, .F. ) ;
#700 = ORIENTED_EDGE ( 'NONE', *, *, #8357, .T. ) ;
#701 = CARTESIAN_POINT ( 'NONE',  ( 0.000000000000000000, 0.000000000000000000, -90.00000000000000000 ) ) ;
#702 = CARTESIAN_POINT ( 'NONE',  ( -45.24999999999994316, 100.0000000000000000, -125.0000000000000000 ) ) ;
#703 = EDGE_CURVE ( 'NONE', #23044, #590, #11400, .T. ) ;
#704 = VECTOR ( 'NONE', #5918, 1000.000000000000114 ) ;
#705 = ADVANCED_FACE ( 'NONE', ( #14000 ), #23134, .F. ) ;
#706 = EDGE_CURVE ( 'NONE', #3521, #2188, #19499, .T. ) ;
#707 = ORIENTED_EDGE ( 'NONE', *, *, #13202, .F. ) ;
#708 = CARTESIAN_POINT ( 'NONE',  ( 45.00000000000004974, -56.79999999999964899, 105.0000000000002132 ) ) ;
#709 = VECTOR ( 'NONE', #15669, 1000.000000000000000 ) ;
#710 = CARTESIAN_POINT ( 'NONE',  ( -24.99999999999998224, -1000.000000000000000, 145.0000119999999697 ) ) ;
#711 = VERTEX_POINT ( 'NONE', #17367 ) ;
#712 = LINE ( 'NONE', #4213, #4849 ) ;
#713 = EDGE_CURVE ( 'NONE', #9956, #13794, #10236, .T. ) ;
#714 = ORIENTED_EDGE ( 'NONE', *, *, #23299, .F. ) ;
#715 = DIRECTION ( 'NONE',  ( 1.000000000000000000, 0.000000000000000000, 0.000000000000000000 ) ) ;
#716 = ORIENTED_EDGE ( 'NONE', *, *, #17409, .T. ) ;
#717 = ORIENTED_EDGE ( 'NONE', *, *, #4723, .F. ) ;
#718 = LINE ( 'NONE', #21363, #15052 ) ;
#719 = AXIS2_PLACEMENT_3D ( 'NONE', #14243, #1403, #19754 ) ;
#720 = DIRECTION ( 'NONE',  ( 1.000000000000000000, 0.000000000000000000, 0.000000000000000000 ) ) ;
#721 = VECTOR ( 'NONE', #17814, 1000.000000000000000 ) ;
#722 = AXIS2_PLACEMENT_3D ( 'NONE', #1603, #20182, #21658 ) ;
#723 = CIRCLE ( 'NONE', #22695, 0.3000000000000016542 ) ;
#724 = LINE ( 'NONE', #11387, #3443 ) ;
#725 = AXIS2_PLACEMENT_3D ( 'NONE', #17069, #2691, #22955 ) ;
#726 = DIRECTION ( 'NONE',  ( 1.000000000000000000, -0.000000000000000000, 6.982962677686266711E-15 ) ) ;
#727 = ORIENTED_EDGE ( 'NONE', *, *, #5522, .F. ) ;
#728 = CARTESIAN_POINT ( 'NONE',  ( 235.0000000000000284, -499.9999999999999432, -59.99999999999997868 ) ) ;
#729 = FILL_AREA_STYLE ('',( #3980 ) ) ;
#730 = CIRCLE ( 'NONE', #10814, 21.02499999999999858 ) ;
#731 = ORIENTED_EDGE ( 'NONE', *, *, #5331, .T. ) ;
#732 = DIRECTION ( 'NONE',  ( -0.000000000000000000, 0.000000000000000000, -1.000000000000000000 ) ) ;
#733 = VERTEX_POINT ( 'NONE', #21327 ) ;
#734 = EDGE_CURVE ( 'NONE', #21032, #15145, #6249, .T. ) ;
#735=STYLED_ITEM('',(#23934),#20017);
#736 = CARTESIAN_POINT ( 'NONE',  ( 0.000000000000000000, -132.2000000000000455, 7.703011046602857601E-15 ) ) ;
#738 = AXIS2_PLACEMENT_3D ( 'NONE', #10187, #23204, #21160 ) ;
#737 = MECHANICAL_DESIGN_GEOMETRIC_PRESENTATION_REPRESENTATION (  '', ( #8859 ), #11190 ) ;
#739 = ORIENTED_EDGE ( 'NONE', *, *, #5618, .F. ) ;
#740 = CIRCLE ( 'NONE', #10410, 2.041999999999999815 ) ;
#741 = LINE ( 'NONE', #6187, #22547 ) ;
#742 = ADVANCED_FACE ( 'NONE', ( #13655 ), #12191, .F. ) ;
#743 = CIRCLE ( 'NONE', #18865, 2.649999999999985700 ) ;
#744 = DIRECTION ( 'NONE',  ( 1.000000000000000000, 0.000000000000000000, 0.000000000000000000 ) ) ;
#745 = COLOUR_RGB ( '',1.000000000000000000, 0.9490196078431372140, 0.9098039215686274384 ) ;
#746 = VECTOR ( 'NONE', #8115, 1000.000000000000000 ) ;
#747 = EDGE_CURVE ( 'NONE', #1893, #4175, #10354, .T. ) ;
#748 = VERTEX_POINT ( 'NONE', #19617 ) ;
#749 = CARTESIAN_POINT ( 'NONE',  ( -280.4976310729379065, 272.3436892194421262, 147.6188186979287025 ) ) ;
#750 = CARTESIAN_POINT ( 'NONE',  ( -127.9021285790841205, 87.55595642181886262, 32.50000000000646594 ) ) ;
#751 = ORIENTED_EDGE ( 'NONE', *, *, #3968, .T. ) ;
#752 = ADVANCED_FACE ( 'NONE', ( #913 ), #15562, .F. ) ;
#753 = UNCERTAINTY_MEASURE_WITH_UNIT (LENGTH_MEASURE( 1.000000000000000082E-05 ), #23433, 'distance_accuracy_value', 'NONE');
#754 = FACE_OUTER_BOUND ( 'NONE', #19293, .T. ) ;
#755 = CARTESIAN_POINT ( 'NONE',  ( -16.51661848988935688, -981.1612097654584659, -145.0000000000001137 ) ) ;
#756 = DIRECTION ( 'NONE',  ( 1.000000000000000000, 0.000000000000000000, 0.000000000000000000 ) ) ;
#757 = CARTESIAN_POINT ( 'NONE',  ( 4.197393957002303999, 7.772902908466098641E-14, -3.503767560748929810 ) ) ;
#758 = ORIENTED_EDGE ( 'NONE', *, *, #16405, .T. ) ;
#760 = AXIS2_PLACEMENT_3D ( 'NONE', #10210, #12066, #20943 ) ;
#759 = AXIS2_PLACEMENT_3D ( 'NONE', #13615, #19105, #17431 ) ;
#761 = CARTESIAN_POINT ( 'NONE',  ( -280.6220388411722411, 271.9822575857424454, -148.2140793454688037 ) ) ;
#762 = CIRCLE ( 'NONE', #20827, 2.499999999999999556 ) ;
#763 = AXIS2_PLACEMENT_3D ( 'NONE', #1583, #22208, #7132 ) ;
#764 = CIRCLE ( 'NONE', #10431, 7.500000000000000888 ) ;
#766 = VERTEX_POINT ( 'NONE', #23002 ) ;
#765 = ORIENTED_EDGE ( 'NONE', *, *, #20200, .T. ) ;
#767 = DIRECTION ( 'NONE',  ( 1.000000000000000000, -1.408839003528726857E-14, -6.982962677686266711E-15 ) ) ;
#768 = CARTESIAN_POINT ( 'NONE',  ( 7.908230272950877549, -3.123266379887881250, -7.776722524729575703 ) ) ;
#769 = LINE ( 'NONE', #1117, #4265 ) ;
#770 = CARTESIAN_POINT ( 'NONE',  ( 284.1582675804705218, 270.9956429438695409, 145.8708543776411943 ) ) ;
#771 = PLANE ( 'NONE',  #4084 ) ;
#772 = ORIENTED_EDGE ( 'NONE', *, *, #4782, .T. ) ;
#773 = DIRECTION ( 'NONE',  ( 0.000000000000000000, 0.000000000000000000, -1.000000000000000000 ) ) ;
#774 = AXIS2_PLACEMENT_3D ( 'NONE', #22101, #9211, #14887 ) ;
#775 = CARTESIAN_POINT ( 'NONE',  ( 45.00000000000000000, 272.9999999999999432, 5.249999999999973355 ) ) ;
#776 =( REPRESENTATION_RELATIONSHIP ('NONE','NONE', #10127, #6236 ) REPRESENTATION_RELATIONSHIP_WITH_TRANSFORMATION ( #273 )SHAPE_REPRESENTATION_RELATIONSHIP( ) );
#777 = CARTESIAN_POINT ( 'NONE',  ( 67.35000000000002274, -112.6666666666666714, 148.0000000000000000 ) ) ;
#778 = PRESENTATION_LAYER_ASSIGNMENT (  '', '', ( #10787 ) ) ;
#779 = TOROIDAL_SURFACE ( 'NONE', #11961, 2.700000000000000622, 0.2000000000000000111 ) ;
#780 = ORIENTED_EDGE ( 'NONE', *, *, #3573, .F. ) ;
#781 = AXIS2_PLACEMENT_3D ( 'NONE', #12948, #7112, #5536 ) ;
#782 = CIRCLE ( 'NONE', #20051, 2.499999999999998668 ) ;
#783 = CARTESIAN_POINT ( 'NONE',  ( 89.00000000000000000, -74.99999999999998579, 3.000000000000000000 ) ) ;
#784 = VERTEX_POINT ( 'NONE', #15907 ) ;
#785 = DIRECTION ( 'NONE',  ( 0.000000000000000000, -0.4999999999999989453, 0.8660254037844391517 ) ) ;
#786 = LINE ( 'NONE', #9977, #23718 ) ;
#787 = EDGE_CURVE ( 'NONE', #23122, #3613, #19452, .T. ) ;
#788 = ADVANCED_FACE ( 'NONE', ( #20967 ), #6715, .F. ) ;
#789 = ORIENTED_EDGE ( 'NONE', *, *, #19625, .F. ) ;
#790 = EDGE_CURVE ( 'NONE', #2904, #12317, #6354, .T. ) ;
#791 = CARTESIAN_POINT ( 'NONE',  ( -15.25452100743371275, 19.87444003246448077, -145.0000000000000000 ) ) ;
#792 = ORIENTED_EDGE ( 'NONE', *, *, #21842, .T. ) ;
#793 = FILL_AREA_STYLE_COLOUR ( '', #3811 ) ;
#794 = CARTESIAN_POINT ( 'NONE',  ( -135.7895026000616951, -1074.740959209979792, -32.49999999999351985 ) ) ;
#795 = LINE ( 'NONE', #16220, #3817 ) ;
#796 = DIRECTION ( 'NONE',  ( 0.000000000000000000, 0.000000000000000000, 1.000000000000000000 ) ) ;
#797 = FACE_OUTER_BOUND ( 'NONE', #2972, .T. ) ;
#798 = CYLINDRICAL_SURFACE ( 'NONE', #13137, 20.00000000000000000 ) ;
#799 = DIRECTION ( 'NONE',  ( 0.000000000000000000, 0.000000000000000000, 1.000000000000000000 ) ) ;
#800 = ORIENTED_EDGE ( 'NONE', *, *, #9748, .T. ) ;
#801 = CARTESIAN_POINT ( 'NONE',  ( 2.500000000000000000, 2.357898499370431722, -2.818925648462311528E-15 ) ) ;
#802 = DIRECTION ( 'NONE',  ( -1.350636282998972974E-14, 0.000000000000000000, -1.000000000000000000 ) ) ;
#803 = DIRECTION ( 'NONE',  ( 1.110223024625157172E-14, 0.000000000000000000, -1.000000000000000000 ) ) ;
#804 = ORIENTED_EDGE ( 'NONE', *, *, #13825, .T. ) ;
#805 = ORIENTED_EDGE ( 'NONE', *, *, #3197, .T. ) ;
#806 = CARTESIAN_POINT ( 'NONE',  ( -69.99999999999997158, -87.33333333333338544, 3.000000000000000000 ) ) ;
#807 = DIRECTION ( 'NONE',  ( 0.000000000000000000, -0.000000000000000000, 1.000000000000000000 ) ) ;
#809 = CARTESIAN_POINT ( 'NONE',  ( -20.63749999999999574, 0.000000000000000000, -23.97500000000000497 ) ) ;
#808 = PRODUCT_DEFINITION_SHAPE ( 'NONE', 'NONE',  #23873 ) ;
#810 = CARTESIAN_POINT ( 'NONE',  ( -79.99999999999995737, -62.00000000000004263, 0.000000000000000000 ) ) ;
#811 = CARTESIAN_POINT ( 'NONE',  ( 160.0000000000000000, 1.959434878635765210E-14, 100.0000000000000000 ) ) ;
#812 = DIRECTION ( 'NONE',  ( 0.000000000000000000, 0.000000000000000000, -1.000000000000000000 ) ) ;
#813 = ORIENTED_EDGE ( 'NONE', *, *, #10441, .T. ) ;
#814 = DIRECTION ( 'NONE',  ( -1.000000000000000000, -3.469446951953613696E-16, 0.000000000000000000 ) ) ;
#815 = DIRECTION ( 'NONE',  ( -1.000000000000000000, -0.000000000000000000, -0.000000000000000000 ) ) ;
#816 = ADVANCED_FACE ( 'NONE', ( #4674 ), #21087, .F. ) ;
#817 = ORIENTED_EDGE ( 'NONE', *, *, #14063, .T. ) ;
#818 = FACE_BOUND ( 'NONE', #20184, .T. ) ;
#819 = ITEM_DEFINED_TRANSFORMATION ( 'NONE', 'NONE', #2693,  #11210 ) ;
#820 = ADVANCED_FACE ( 'NONE', ( #17468 ), #12087, .T. ) ;
#821 = LINE ( 'NONE', #19284, #1182 ) ;
#822 = DIRECTION ( 'NONE',  ( 0.000000000000000000, -1.000000000000000000, -3.172065784643303781E-15 ) ) ;
#823 = CARTESIAN_POINT ( 'NONE',  ( -280.0000000000000568, 272.9999999999999432, 145.0000000000000284 ) ) ;
#824 = UNCERTAINTY_MEASURE_WITH_UNIT (LENGTH_MEASURE( 1.000000000000000082E-05 ), #13578, 'distance_accuracy_value', 'NONE');
#825 = EDGE_LOOP ( 'NONE', ( #14289, #18811, #20424, #21702 ) ) ;
#826 = ORIENTED_EDGE ( 'NONE', *, *, #2161, .F. ) ;
#827 = PLANE ( 'NONE',  #4915 ) ;
#828 = DIRECTION ( 'NONE',  ( 0.000000000000000000, 0.000000000000000000, -1.000000000000000000 ) ) ;
#829 = VERTEX_POINT ( 'NONE', #1392 ) ;
#830 = ORIENTED_EDGE ( 'NONE', *, *, #12374, .F. ) ;
#831 = CYLINDRICAL_SURFACE ( 'NONE', #5609, 7.500000000000007105 ) ;
#832 = LINE ( 'NONE', #21116, #18019 ) ;
#833 = ORIENTED_EDGE ( 'NONE', *, *, #925, .F. ) ;
#834 = CARTESIAN_POINT ( 'NONE',  ( -134.7167544493340472, -1076.657711551589273, -28.73951976925632223 ) ) ;
#835 = EDGE_CURVE ( 'NONE', #2765, #10209, #1509, .T. ) ;
#836 = ORIENTED_EDGE ( 'NONE', *, *, #6196, .T. ) ;
#837 = LINE ( 'NONE', #8216, #5993 ) ;
#838 = DIRECTION ( 'NONE',  ( 1.000000000000000000, 0.000000000000000000, -0.000000000000000000 ) ) ;
#839 = EDGE_LOOP ( 'NONE', ( #4051, #13336, #850, #10609, #14408 ) ) ;
#840 = VERTEX_POINT ( 'NONE', #23717 ) ;
#841 = CARTESIAN_POINT ( 'NONE',  ( 2.836893136758676270, 3.208949435745843903, -3.505054077164911241 ) ) ;
#842 = CARTESIAN_POINT ( 'NONE',  ( -20.63749999999999574, 3.061616997868383043E-15, 25.00000000000000000 ) ) ;
#843 = EDGE_CURVE ( 'NONE', #22443, #6335, #8908, .T. ) ;
#844 = CARTESIAN_POINT ( 'NONE',  ( 0.000000000000000000, 0.000000000000000000, 4.000000000000000000 ) ) ;
#845 = DIRECTION ( 'NONE',  ( 0.000000000000000000, 0.000000000000000000, -1.000000000000000000 ) ) ;
#846 = VERTEX_POINT ( 'NONE', #23494 ) ;
#847 = CARTESIAN_POINT ( 'NONE',  ( -7.968863443239230016, -4.547634245050486079, -8.057411785091789014 ) ) ;
#848 = SURFACE_STYLE_USAGE ( .BOTH. , #23054 ) ;
#849 = EDGE_CURVE ( 'NONE', #11269, #12933, #5576, .T. ) ;
#850 = ORIENTED_EDGE ( 'NONE', *, *, #20757, .T. ) ;
#851 = VECTOR ( 'NONE', #20972, 1000.000000000000000 ) ;
#852 = VERTEX_POINT ( 'NONE', #10959 ) ;
#853 = CARTESIAN_POINT ( 'NONE',  ( 16.51667796972429514, -18.83873075115305440, -145.0000000000000000 ) ) ;
#854 = ORIENTED_EDGE ( 'NONE', *, *, #6766, .T. ) ;
#855 = DIRECTION ( 'NONE',  ( -1.000000000000000000, -0.000000000000000000, -0.000000000000000000 ) ) ;
#856 = CARTESIAN_POINT ( 'NONE',  ( 37.61698748598423947, 140.0355749532214702, -90.00000000000000000 ) ) ;
#857 = ORIENTED_EDGE ( 'NONE', *, *, #7014, .T. ) ;
#858 = CARTESIAN_POINT ( 'NONE',  ( -281.2440776823446527, 269.1689414351989740, 150.0938770989752982 ) ) ;
#859 = DIRECTION ( 'NONE',  ( -1.000000000000000000, -2.775557561562891351E-17, 0.000000000000000000 ) ) ;
#860 = ORIENTED_EDGE ( 'NONE', *, *, #4723, .T. ) ;
#861 = ADVANCED_FACE ( 'NONE', ( #22030 ), #21930, .F. ) ;
#862 = FACE_BOUND ( 'NONE', #14300, .T. ) ;
#863 = EDGE_CURVE ( 'NONE', #1754, #12819, #21567, .T. ) ;
#864 = CARTESIAN_POINT ( 'NONE',  ( -24.19933745276217252, -993.5122599704404820, -145.0000000000001137 ) ) ;
#865 = DIRECTION ( 'NONE',  ( 0.000000000000000000, 0.000000000000000000, -1.000000000000000000 ) ) ;
#866 = AXIS2_PLACEMENT_3D ( 'NONE', #22309, #11621, #11359 ) ;
#867 = FACE_OUTER_BOUND ( 'NONE', #11588, .T. ) ;
#868 = ORIENTED_EDGE ( 'NONE', *, *, #19695, .F. ) ;
#869 = CARTESIAN_POINT ( 'NONE',  ( -7.499999999999999112, 41.99999999999998579, -100.0000000000000000 ) ) ;
#870 = CONTEXT_DEPENDENT_SHAPE_REPRESENTATION ( #9106, #1391 ) ;
#871 = EDGE_CURVE ( 'NONE', #8499, #16240, #17927, .T. ) ;
#872 = EDGE_CURVE ( 'NONE', #15992, #2924, #11012, .T. ) ;
#874 = VERTEX_POINT ( 'NONE', #16724 ) ;
#873 = ORIENTED_EDGE ( 'NONE', *, *, #18205, .T. ) ;
#875 = CARTESIAN_POINT ( 'NONE',  ( -145.2408737859505834, -1078.096661784570870, -29.99999999999344880 ) ) ;
#876 = CARTESIAN_POINT ( 'NONE',  ( 7.500000000000000000, 1.572594658376109011, -7.069792055233639516 ) ) ;
#877 = DIRECTION ( 'NONE',  ( 0.000000000000000000, 0.000000000000000000, -1.000000000000000000 ) ) ;
#878 = DIRECTION ( 'NONE',  ( -0.000000000000000000, -0.000000000000000000, 1.000000000000000000 ) ) ;
#879 = FACE_OUTER_BOUND ( 'NONE', #17446, .T. ) ;
#880 = VERTEX_POINT ( 'NONE', #13468 ) ;
#881 = CIRCLE ( 'NONE', #521, 2.700000000000000622 ) ;
#882 = CARTESIAN_POINT ( 'NONE',  ( -44.80746418436648071, -137.9031948627975908, -90.00000000000000000 ) ) ;
#883 = FACE_BOUND ( 'NONE', #18234, .T. ) ;
#884 = LINE ( 'NONE', #23340, #6165 ) ;
#885 = VERTEX_POINT ( 'NONE', #4487 ) ;
#886 = FACE_OUTER_BOUND ( 'NONE', #15033, .T. ) ;
#887 = ORIENTED_EDGE ( 'NONE', *, *, #20314, .T. ) ;
#888 = CYLINDRICAL_SURFACE ( 'NONE', #2282, 20.00000000000000000 ) ;
#889 = DIRECTION ( 'NONE',  ( 0.000000000000000000, 0.000000000000000000, 1.000000000000000000 ) ) ;
#890 = ORIENTED_EDGE ( 'NONE', *, *, #22306, .T. ) ;
#891 = CARTESIAN_POINT ( 'NONE',  ( -21.69892645963121325, 12.52401366518118841, -145.0000000000000000 ) ) ;
#892 = ORIENTED_EDGE ( 'NONE', *, *, #1894, .F. ) ;
#893 = DIRECTION ( 'NONE',  ( -1.000000000000000000, -0.000000000000000000, -0.000000000000000000 ) ) ;
#894 = DIRECTION ( 'NONE',  ( 0.000000000000000000, -1.000000000000000000, 3.392348130799088816E-15 ) ) ;
#895 = VECTOR ( 'NONE', #10102, 1000.000000000000000 ) ;
#896 = MECHANICAL_DESIGN_GEOMETRIC_PRESENTATION_REPRESENTATION (  '', ( #6700 ), #10991 ) ;
#897 = CARTESIAN_POINT ( 'NONE',  ( 0.000000000000000000, -130.5567675943147492, -0.000000000000000000 ) ) ;
#898 = EDGE_CURVE ( 'NONE', #14701, #7954, #741, .T. ) ;
#899 = CARTESIAN_POINT ( 'NONE',  ( 281.7502846751310699, 269.1405375976306686, 145.8716261326570702 ) ) ;
#900 = DIRECTION ( 'NONE',  ( 0.7071067811865320296, 8.659560562355062281E-17, 0.7071067811865631159 ) ) ;
#901 = EDGE_CURVE ( 'NONE', #19530, #15233, #571, .T. ) ;
#902 = FACE_OUTER_BOUND ( 'NONE', #12806, .T. ) ;
#903 = ORIENTED_EDGE ( 'NONE', *, *, #3665, .F. ) ;
#904 = EDGE_CURVE ( 'NONE', #15698, #12205, #4249, .T. ) ;
#905 = DIRECTION ( 'NONE',  ( 0.000000000000000000, -1.000000000000000000, 0.000000000000000000 ) ) ;
#906 = CYLINDRICAL_SURFACE ( 'NONE', #17761, 145.0000000000000284 ) ;
#907 = VERTEX_POINT ( 'NONE', #17295 ) ;
#908 = ORIENTED_EDGE ( 'NONE', *, *, #12705, .F. ) ;
#909 = DIRECTION ( 'NONE',  ( 0.000000000000000000, 0.000000000000000000, 1.000000000000000000 ) ) ;
#910 = CARTESIAN_POINT ( 'NONE',  ( 145.0000000000000284, 0.000000000000000000, -90.00000000000000000 ) ) ;
#911 = ADVANCED_FACE ( 'NONE', ( #9367 ), #17415, .F. ) ;
#912 = EDGE_CURVE ( 'NONE', #1785, #23190, #20909, .T. ) ;
#913 = FACE_OUTER_BOUND ( 'NONE', #11726, .T. ) ;
#914 = AXIS2_PLACEMENT_3D ( 'NONE', #2286, #9683, #4344 ) ;
#915 = CIRCLE ( 'NONE', #6313, 7.500000000000001776 ) ;
#916 = FACE_BOUND ( 'NONE', #6482, .T. ) ;
#917 = DIRECTION ( 'NONE',  ( 1.000000000000000000, 0.000000000000000000, 0.000000000000000000 ) ) ;
#918 = DIRECTION ( 'NONE',  ( 1.000000000000000000, -0.000000000000000000, -0.000000000000000000 ) ) ;
#919 = ORIENTED_EDGE ( 'NONE', *, *, #5943, .T. ) ;
#920 = CARTESIAN_POINT ( 'NONE',  ( 0.000000000000000000, -1.178949249685213863, 2.042000000000002924 ) ) ;
#921 = CARTESIAN_POINT ( 'NONE',  ( 7.497491405671719455, 144.8060344827586334, 90.00000000000000000 ) ) ;
#922 = DIRECTION ( 'NONE',  ( 0.000000000000000000, 0.5000000000000009992, 0.8660254037844380415 ) ) ;
#923 = ORIENTED_EDGE ( 'NONE', *, *, #16478, .F. ) ;
#924 = DIRECTION ( 'NONE',  ( -1.000000000000000000, 1.408839003528726857E-14, 6.982962677686266711E-15 ) ) ;
#925 = EDGE_CURVE ( 'NONE', #23462, #21875, #23659, .T. ) ;
#926 = CARTESIAN_POINT ( 'NONE',  ( 0.000000000000000000, 0.000000000000000000, 138.9999999999999716 ) ) ;
#927 = CARTESIAN_POINT ( 'NONE',  ( -146.0000000000000568, -784.4690652294805204, 32.05500000000641592 ) ) ;
#928 = DIRECTION ( 'NONE',  ( -1.000000000000000000, 1.224646799147354686E-16, 0.000000000000000000 ) ) ;
#929 = EDGE_LOOP ( 'NONE', ( #19445, #20802, #6754, #17160, #13863 ) ) ;
#930 = CIRCLE ( 'NONE', #16749, 5.249999999999949374 ) ;
#931 = VERTEX_POINT ( 'NONE', #630 ) ;
#932 = DIRECTION ( 'NONE',  ( 0.000000000000000000, 0.000000000000000000, -1.000000000000000000 ) ) ;
#933 = CARTESIAN_POINT ( 'NONE',  ( 280.2481149223240209, 269.9433523009094529, 145.5743436287470161 ) ) ;
#934 = ORIENTED_EDGE ( 'NONE', *, *, #20472, .F. ) ;
#935 = AXIS2_PLACEMENT_3D ( 'NONE', #10391, #13792, #16052 ) ;
#936 = ADVANCED_FACE ( 'NONE', ( #18395 ), #22829, .T. ) ;
#937 = EDGE_CURVE ( 'NONE', #19800, #4863, #16618, .T. ) ;
#938 = ORIENTED_EDGE ( 'NONE', *, *, #5830, .F. ) ;
#939 = DIRECTION ( 'NONE',  ( 1.000000000000000000, -0.000000000000000000, -0.000000000000000000 ) ) ;
#940 = EDGE_CURVE ( 'NONE', #17429, #3770, #2550, .T. ) ;
#941 = CARTESIAN_POINT ( 'NONE',  ( -127.9021285790841205, 87.55595642181886262, 32.50000000000646594 ) ) ;
#943 = ORIENTED_EDGE ( 'NONE', *, *, #1344, .F. ) ;
#942 = CIRCLE ( 'NONE', #6346, 2.500000000000002220 ) ;
#944 = CARTESIAN_POINT ( 'NONE',  ( -135.2464651929980164, -1075.719328653694674, -32.24903484778816676 ) ) ;
#945 = ORIENTED_EDGE ( 'NONE', *, *, #15780, .T. ) ;
#946 = CONICAL_SURFACE ( 'NONE', #22543, 2.055000000000001492, 0.7853981633974633780 ) ;
#947 = LINE ( 'NONE', #17750, #601 ) ;
#948 = CYLINDRICAL_SURFACE ( 'NONE', #18630, 2.649999999999985700 ) ;
#949 = VERTEX_POINT ( 'NONE', #11659 ) ;
#950 = ORIENTED_EDGE ( 'NONE', *, *, #15583, .F. ) ;
#951 = CARTESIAN_POINT ( 'NONE',  ( 133.6256533058505340, 78.54427823740819292, -31.99339931332764664 ) ) ;
#952 = AXIS2_PLACEMENT_3D ( 'NONE', #10071, #9939, #18964 ) ;
#953 = CARTESIAN_POINT ( 'NONE',  ( 0.6640947660595348800, -4.471078309994175548, -3.602146406945708090 ) ) ;
#954 = DIRECTION ( 'NONE',  ( -1.000000000000000000, -0.000000000000000000, -0.000000000000000000 ) ) ;
#955 = PLANE ( 'NONE',  #7810 ) ;
#956 = ORIENTED_EDGE ( 'NONE', *, *, #20313, .F. ) ;
#957 = FACE_OUTER_BOUND ( 'NONE', #21689, .T. ) ;
#958 = CIRCLE ( 'NONE', #17951, 2.649999999999999467 ) ;
#959 =( LENGTH_UNIT ( ) NAMED_UNIT ( * ) SI_UNIT ( .MILLI., .METRE. ) );
#960 = AXIS2_PLACEMENT_3D ( 'NONE', #15591, #5069, #17857 ) ;
#961 = ORIENTED_EDGE ( 'NONE', *, *, #22708, .T. ) ;
#962 =( GEOMETRIC_REPRESENTATION_CONTEXT ( 3 ) GLOBAL_UNCERTAINTY_ASSIGNED_CONTEXT ( ( #11735 ) ) GLOBAL_UNIT_ASSIGNED_CONTEXT ( ( #18533, #303, #5615 ) ) REPRESENTATION_CONTEXT ( 'NONE', 'WORKASPACE' ) );
#963 = VERTEX_POINT ( 'NONE', #1980 ) ;
#964 = CLOSED_SHELL ( 'NONE', ( #4303, #1614, #4833, #820, #19092, #13292, #16891, #6525, #17781, #936, #12661, #23313, #19770, #2931, #21369, #16177, #3125, #20181, #11405, #2100, #13635, #20040, #9767, #13206, #11995, #1311, #13323 ) ) ;
#965 = CARTESIAN_POINT ( 'NONE',  ( -23.72540896994113524, -8.050072860292576848, -145.0000000000000000 ) ) ;
#966 = ORIENTED_EDGE ( 'NONE', *, *, #21059, .F. ) ;
#967 = CARTESIAN_POINT ( 'NONE',  ( 281.4928932188133217, -127.0000000000000568, 152.4000000000014268 ) ) ;
#968 = LINE ( 'NONE', #19434, #7526 ) ;
#969 = ORIENTED_EDGE ( 'NONE', *, *, #12126, .F. ) ;
#970 = AXIS2_PLACEMENT_3D ( 'NONE', #14005, #15567, #10496 ) ;
#971 = CARTESIAN_POINT ( 'NONE',  ( -281.2440776823446527, 268.3758453455903918, 147.1427398886702917 ) ) ;
#972 = LINE ( 'NONE', #15862, #14857 ) ;
#973 = ORIENTED_EDGE ( 'NONE', *, *, #1611, .T. ) ;
#974 = DIRECTION ( 'NONE',  ( -1.000000000000000000, -3.469446951953617640E-16, -8.673617379884035472E-17 ) ) ;
#975 = CARTESIAN_POINT ( 'NONE',  ( -1.642023387942652235, -975.0000492607058504, -145.0000000000001421 ) ) ;
#976 = CARTESIAN_POINT ( 'NONE',  ( 0.000000000000000000, 0.000000000000000000, -90.00000000000000000 ) ) ;
#977 = AXIS2_PLACEMENT_3D ( 'NONE', #2583, #10105, #18756 ) ;
#978 = LINE ( 'NONE', #17529, #19608 ) ;
#979 = ORIENTED_EDGE ( 'NONE', *, *, #3400, .T. ) ;
#980 = CARTESIAN_POINT ( 'NONE',  ( 50.00000000000000000, 0.000000000000000000, 0.000000000000000000 ) ) ;
#981 = SURFACE_STYLE_USAGE ( .BOTH. , #17532 ) ;
#982 = PRODUCT_DEFINITION_SHAPE ( 'NONE', 'NONE',  #23842 ) ;
#984 = EDGE_LOOP ( 'NONE', ( #10266, #7109, #23635, #16321 ) ) ;
#983 = EDGE_LOOP ( 'NONE', ( #16297, #10058, #10495 ) ) ;
#985 = DIRECTION ( 'NONE',  ( -6.982962677686266711E-15, 9.837870180509810443E-29, -1.000000000000000000 ) ) ;
#986 = FACE_OUTER_BOUND ( 'NONE', #1753, .T. ) ;
#987 = AXIS2_PLACEMENT_3D ( 'NONE', #1859, #16486, #13027 ) ;
#988 = CARTESIAN_POINT ( 'NONE',  ( -281.4928932188134922, -127.0000000000000568, -150.2000000000013245 ) ) ;
#989 = DIRECTION ( 'NONE',  ( 0.000000000000000000, 0.000000000000000000, 1.000000000000000000 ) ) ;
#990 = CARTESIAN_POINT ( 'NONE',  ( -281.4928932188135491, -132.2000000000000455, 177.2000000000014097 ) ) ;
#991 = EDGE_CURVE ( 'NONE', #20344, #17672, #1333, .T. ) ;
#992 = CARTESIAN_POINT ( 'NONE',  ( -155.0000000000000284, -784.4690652294804067, 30.00000000000648015 ) ) ;
#993 = EDGE_LOOP ( 'NONE', ( #23590, #14200 ) ) ;
#994 = EDGE_CURVE ( 'NONE', #13225, #7372, #14096, .T. ) ;
#995 = EDGE_CURVE ( 'NONE', #20571, #18758, #14923, .T. ) ;
#996 = LINE ( 'NONE', #12058, #1812 ) ;
#997 = B_SPLINE_CURVE_WITH_KNOTS ( 'NONE', 3,
 ( #16561, #14521, #9199, #21855, #11385, #5449, #16437, #14640, #23787, #12745, #3867, #5814, #18479, #16679, #5326, #16789, #14756, #7484, #18699, #20277, #9325, #7604, #12857, #28, #20057, #10914, #18236, #9077, #14997, #13218, #20519, #22087, #3732, #7245 ),
 .UNSPECIFIED., .F., .F.,
 ( 4, 2, 2, 2, 2, 2, 2, 2, 2, 2, 2, 2, 2, 2, 2, 2, 4 ),
 ( 0.5000000000000000000, 0.5312500000000000000, 0.5625000000000000000, 0.5937500000000000000, 0.6250000000000000000, 0.6562500000000000000, 0.6875000000000000000, 0.7187500000000000000, 0.7500000000000000000, 0.7812500000000000000, 0.8125000000000000000, 0.8437500000000000000, 0.8750000000000000000, 0.9062500000000000000, 0.9375000000000000000, 0.9687500000000000000, 1.000000000000000000 ),
 .UNSPECIFIED. ) ;
#998 = FACE_OUTER_BOUND ( 'NONE', #17064, .T. ) ;
#999 = EDGE_CURVE ( 'NONE', #6769, #306, #21098, .T. ) ;
#1000 = ORIENTED_EDGE ( 'NONE', *, *, #10407, .F. ) ;
#1001 = FACE_OUTER_BOUND ( 'NONE', #4174, .T. ) ;
#1002 = ORIENTED_EDGE ( 'NONE', *, *, #5522, .T. ) ;
#1003 = DIRECTION ( 'NONE',  ( 0.000000000000000000, 1.000000000000000000, 0.000000000000000000 ) ) ;
#1004 = DIRECTION ( 'NONE',  ( 1.000000000000000000, 0.000000000000000000, 0.000000000000000000 ) ) ;
#1005 = ORIENTED_EDGE ( 'NONE', *, *, #16733, .T. ) ;
#1006 = VECTOR ( 'NONE', #14424, 1000.000000000000000 ) ;
#1007 = CARTESIAN_POINT ( 'NONE',  ( 6.487740029101478179, 24.19933745276211212, -145.0000000000000000 ) ) ;
#1008 = CYLINDRICAL_SURFACE ( 'NONE', #22278, 2.649999999999985700 ) ;
#1009 = DIRECTION ( 'NONE',  ( 0.000000000000000000, 0.000000000000000000, 1.000000000000000000 ) ) ;
#1010 = VECTOR ( 'NONE', #22140, 1000.000000000000114 ) ;
#1011 = CARTESIAN_POINT ( 'NONE',  ( -100.0000000000001137, -129.2000000000000455, 7.690461757479017101E-15 ) ) ;
#1012 = CARTESIAN_POINT ( 'NONE',  ( 3.096526599377912525, -6.872473572140722631, -5.976664475826341615E-15 ) ) ;
#1013 = DIRECTION ( 'NONE',  ( -0.7232617928448825673, 0.6905739489807055653, 6.982962677686266711E-15 ) ) ;
#1014 = ORIENTED_EDGE ( 'NONE', *, *, #14681, .T. ) ;
#1015 = FACE_OUTER_BOUND ( 'NONE', #12354, .T. ) ;
#1016 = DIRECTION ( 'NONE',  ( -0.000000000000000000, -0.000000000000000000, 1.000000000000000000 ) ) ;
#1017 = B_SPLINE_CURVE_WITH_KNOTS ( 'NONE', 3,
 ( #1766, #14723, #19115, #11107, #18876 ),
 .UNSPECIFIED., .F., .F.,
 ( 4, 1, 4 ),
 ( 0.000000000000000000, 0.002309401076758506657, 0.004618802153517013315 ),
 .UNSPECIFIED. ) ;
#1018 = AXIS2_PLACEMENT_3D ( 'NONE', #15491, #15361, #9695 ) ;
#1019 = ORIENTED_EDGE ( 'NONE', *, *, #13645, .T. ) ;
#1020 = ORIENTED_EDGE ( 'NONE', *, *, #23692, .T. ) ;
#1021 = CARTESIAN_POINT ( 'NONE',  ( 285.2000000000013529, -129.2000000000000455, 146.4928932188134638 ) ) ;
#1022 = CYLINDRICAL_SURFACE ( 'NONE', #9203, 25.00000000000000000 ) ;
#1023 = VECTOR ( 'NONE', #21634, 1000.000000000000000 ) ;
#1024 = LINE ( 'NONE', #809, #15629 ) ;
#1025 = EDGE_CURVE ( 'NONE', #6490, #3871, #4720, .T. ) ;
#1026 = CARTESIAN_POINT ( 'NONE',  ( 132.1831532210145781, 80.94878845338391216, 32.18904844917290831 ) ) ;
#1027 = FACE_OUTER_BOUND ( 'NONE', #543, .T. ) ;
#1028 = EDGE_CURVE ( 'NONE', #3982, #8260, #19323, .T. ) ;
#1029 = DIRECTION ( 'NONE',  ( 1.000000000000000000, 0.000000000000000000, 0.000000000000000000 ) ) ;
#1030 = ADVANCED_FACE ( 'NONE', ( #12132 ), #13818, .F. ) ;
#1031 = VERTEX_POINT ( 'NONE', #12386 ) ;
#1032 = DIRECTION ( 'NONE',  ( -0.000000000000000000, -0.000000000000000000, 1.000000000000000000 ) ) ;
#1033 = CARTESIAN_POINT ( 'NONE',  ( -6.259644161404860030E-16, -4.618802153517027165, -3.433295621305388234 ) ) ;
#1034 = CARTESIAN_POINT ( 'NONE',  ( 145.9999999999997726, -209.9999999999996874, 32.05500000000641592 ) ) ;
#1035 = ORIENTED_EDGE ( 'NONE', *, *, #13674, .F. ) ;
#1036 = AXIS2_PLACEMENT_3D ( 'NONE', #479, #16888, #5898 ) ;
#1037 = CARTESIAN_POINT ( 'NONE',  ( 2.500000000000000000, 2.357898499370433054, -1.951563910473907981E-15 ) ) ;
#1038 =( REPRESENTATION_RELATIONSHIP ('NONE','NONE', #10127, #6508 ) REPRESENTATION_RELATIONSHIP_WITH_TRANSFORMATION ( #22856 )SHAPE_REPRESENTATION_RELATIONSHIP( ) );
#1039 = ADVANCED_FACE ( 'NONE', ( #3145 ), #6781, .T. ) ;
#1040 = CARTESIAN_POINT ( 'NONE',  ( 0.000000000000000000, 0.000000000000000000, -90.00000000000000000 ) ) ;
#1041 = CARTESIAN_POINT ( 'NONE',  ( -6.875000000000001776, -4.690970937165714894, -7.298562697733108173 ) ) ;
#1042 = PRODUCT_DEFINITION ( 'UNKNOWN', '', #6177, #18456 ) ;
#1043 = FACE_OUTER_BOUND ( 'NONE', #18088, .T. ) ;
#1045 = VECTOR ( 'NONE', #15936, 999.9999999999998863 ) ;
#1044 = DIRECTION ( 'NONE',  ( 0.000000000000000000, 1.224646799147353207E-16, 1.000000000000000000 ) ) ;
#1046 = EDGE_CURVE ( 'NONE', #4892, #22378, #4610, .T. ) ;
#1047 = DIRECTION ( 'NONE',  ( 1.000000000000000000, 0.000000000000000000, 0.000000000000000000 ) ) ;
#1048 = CIRCLE ( 'NONE', #19178, 4.000000000000000000 ) ;
#1049 = CARTESIAN_POINT ( 'NONE',  ( -285.1663407402830899, 268.4822561791010571, 146.3681929792554399 ) ) ;
#1050 = ORIENTED_EDGE ( 'NONE', *, *, #15908, .T. ) ;
#1051 = ORIENTED_EDGE ( 'NONE', *, *, #650, .F. ) ;
#1052 = B_SPLINE_CURVE_WITH_KNOTS ( 'NONE', 3,
 ( #9232, #278, #22370, #3531, #9350, #10941, #2076, #20438, #7635, #13244, #13126, #18510, #14673, #161, #12780, #11057, #16464, #1716, #20548, #1964, #7407, #412, #3999, #11418, #15149, #2190, #14906, #9583 ),
 .UNSPECIFIED., .F., .F.,
 ( 4, 2, 2, 2, 2, 2, 2, 2, 2, 2, 2, 2, 2, 4 ),
 ( 0.007862850516742138016, 0.008354729399060728881, 0.008846608281379319746, 0.009830366046016465048, 0.01032224492833501775, 0.01081412381065357219, 0.01130600269297213530, 0.01179788157529069667, 0.01278163933992781248, 0.01327351822224636518, 0.01376539710456491789, 0.01425727598688347232, 0.01474915486920202502, 0.01573291263383913910 ),
 .UNSPECIFIED. ) ;
#1053 = CYLINDRICAL_SURFACE ( 'NONE', #6841, 145.0000000000000284 ) ;
#1054 = LINE ( 'NONE', #19399, #20423 ) ;
#1055 = ORIENTED_EDGE ( 'NONE', *, *, #2680, .T. ) ;
#1056 = CARTESIAN_POINT ( 'NONE',  ( 2.500000000000002220, -1.178949249685218970, -2.041999999999998483 ) ) ;
#1057 = CIRCLE ( 'NONE', #23027, 4.250000000000000000 ) ;
#1058 = ORIENTED_EDGE ( 'NONE', *, *, #22905, .F. ) ;
#1059 = DIRECTION ( 'NONE',  ( 0.000000000000000000, 0.000000000000000000, 1.000000000000000000 ) ) ;
#1060 = DIRECTION ( 'NONE',  ( 6.982962677686266711E-15, -9.837870180509810443E-29, 1.000000000000000000 ) ) ;
#1061 = EDGE_LOOP ( 'NONE', ( #11544, #14347, #943, #7992 ) ) ;
#1062 = AXIS2_PLACEMENT_3D ( 'NONE', #23583, #7039, #5346 ) ;
#1063 = CARTESIAN_POINT ( 'NONE',  ( -2.688821387764050996E-14, -4.618802153517012954, -0.4999999999999995559 ) ) ;
#1064 = VECTOR ( 'NONE', #2222, 1000.000000000000114 ) ;
#1065 = AXIS2_PLACEMENT_3D ( 'NONE', #3394, #1596, #4988 ) ;
#1066 = ORIENTED_EDGE ( 'NONE', *, *, #17131, .T. ) ;
#1067 = CYLINDRICAL_SURFACE ( 'NONE', #22936, 145.0000000000000284 ) ;
#1068 = FACE_OUTER_BOUND ( 'NONE', #19426, .T. ) ;
#1069 = EDGE_LOOP ( 'NONE', ( #487, #5225, #6200, #6955 ) ) ;
#1070 = EDGE_LOOP ( 'NONE', ( #5859, #20179, #7990, #3213 ) ) ;
#1071 = CARTESIAN_POINT ( 'NONE',  ( 134.1261853992453723, 77.68633335585815303, -30.32927184981474866 ) ) ;
#1072 = CARTESIAN_POINT ( 'NONE',  ( 1.243802165048773611, -3.900692638707475624, -3.223146290109810241 ) ) ;
#1073 = EDGE_CURVE ( 'NONE', #7880, #21824, #10292, .T. ) ;
#1074 = EDGE_CURVE ( 'NONE', #19239, #3203, #19111, .T. ) ;
#1075 = EDGE_CURVE ( 'NONE', #603, #2349, #20263, .T. ) ;
#1076 = DIRECTION ( 'NONE',  ( -1.000000000000000000, 0.000000000000000000, 0.000000000000000000 ) ) ;
#1077 = CIRCLE ( 'NONE', #20722, 2.649999999999975486 ) ;
#1078 = DIRECTION ( 'NONE',  ( 0.000000000000000000, 0.000000000000000000, -1.000000000000000000 ) ) ;
#1079 = EDGE_LOOP ( 'NONE', ( #23639, #11251, #9429 ) ) ;
#1080 = VECTOR ( 'NONE', #12261, 1000.000000000000000 ) ;
#1081 = DIRECTION ( 'NONE',  ( 1.000000000000000000, 3.736327486719276364E-16, 1.067522139062650425E-16 ) ) ;
#1082 = CIRCLE ( 'NONE', #18429, 23.50000000000000000 ) ;
#1083 = VECTOR ( 'NONE', #9378, 1000.000000000000000 ) ;
#1084 = AXIS2_PLACEMENT_3D ( 'NONE', #6713, #12312, #4901 ) ;
#1085 = ORIENTED_EDGE ( 'NONE', *, *, #2157, .T. ) ;
#1086 = ORIENTED_EDGE ( 'NONE', *, *, #14681, .F. ) ;
#1087 = B_SPLINE_CURVE_WITH_KNOTS ( 'NONE', 3,
 ( #11660, #265, #22590, #2179, #6054, #2428, #631, #20787, #11774, #19083, #2552, #18965, #5699, #16697, #13235, #7624, #22361, #15016, #20427, #4250 ),
 .UNSPECIFIED., .F., .F.,
 ( 4, 2, 2, 2, 2, 2, 2, 2, 2, 4 ),
 ( 0.000000000000000000, 0.001035985217005840064, 0.002071970434011680129, 0.003107955651017520193, 0.003625948259520417674, 0.004143940868023315155, 0.005179926085028993023, 0.006215911302034670891, 0.007251896519040349626, 0.008287881736046026626 ),
 .UNSPECIFIED. ) ;
#1088 = CARTESIAN_POINT ( 'NONE',  ( 12.52399064345484980, -21.69904058272398117, -145.0000000000000000 ) ) ;
#1089 = ORIENTED_EDGE ( 'NONE', *, *, #14740, .T. ) ;
#1090 = DIRECTION ( 'NONE',  ( 1.000000000000000000, 3.469446951953598905E-16, -4.625929269271499719E-16 ) ) ;
#1091 = CARTESIAN_POINT ( 'NONE',  ( -44.80746418436748968, 137.9031948627972781, 90.00000000000000000 ) ) ;
#1092 = ORIENTED_EDGE ( 'NONE', *, *, #7396, .F. ) ;
#1093 = B_SPLINE_SURFACE_WITH_KNOTS ( 'NONE', 1, 3, ( 
 ( #5953, #2443, #17190, #3899, #761, #22488, #15389, #11788, #13611, #5842 ),
 ( #8012, #9835, #15273, #22379, #13362, #18733, #9472, #5713, #22605, #11672 ),
 ( #9589, #421, #7890, #13250, #20553, #4129, #284, #17313, #15155, #7774 ),
 ( #20804, #4007, #11424, #15036, #20921, #8143, #20674, #2194, #641, #16953 ) ),
 .UNSPECIFIED., .F., .F., .F.,
 ( 2, 1, 1, 2 ),
 ( 4, 2, 2, 2, 4 ),
 ( -0.01000000000000000021, 0.000000000000000000, 1.000000000000000000, 1.010099999999999998 ),
 ( 0.000000000000000000, 0.2500000000000000000, 0.5000000000000000000, 0.7500000000000000000, 1.000000000000000000 ),
 .UNSPECIFIED. ) ;
#1094 = VECTOR ( 'NONE', #15458, 1000.000000000000000 ) ;
#1095 = AXIS2_PLACEMENT_3D ( 'NONE', #9625, #16992, #2360 ) ;
#1096 = DIRECTION ( 'NONE',  ( 1.000000000000000000, 0.000000000000000000, 0.000000000000000000 ) ) ;
#1097 = CARTESIAN_POINT ( 'NONE',  ( 25.00000000000001421, -37.41657386773940885, 125.0000000000001705 ) ) ;
#1098 = VECTOR ( 'NONE', #7006, 1000.000000000000000 ) ;
#1099 = ORIENTED_EDGE ( 'NONE', *, *, #23146, .F. ) ;
#1100 = VECTOR ( 'NONE', #136, 1000.000000000000000 ) ;
#1101 = DIRECTION ( 'NONE',  ( 3.202566417187928841E-16, -1.000000000000000000, 3.469446951953614583E-15 ) ) ;
#1102 = CARTESIAN_POINT ( 'NONE',  ( -281.4928932188135491, 267.7999999999999545, 147.1999999999999886 ) ) ;
#1103 = VECTOR ( 'NONE', #4319, 1000.000000000000000 ) ;
#1104 = DIRECTION ( 'NONE',  ( 0.000000000000000000, 0.000000000000000000, -1.000000000000000000 ) ) ;
#1105 = DIRECTION ( 'NONE',  ( -0.000000000000000000, -1.000000000000000000, -0.000000000000000000 ) ) ;
#1106 = ORIENTED_EDGE ( 'NONE', *, *, #5078, .F. ) ;
#1107 = DIRECTION ( 'NONE',  ( 1.000000000000000000, -0.000000000000000000, 6.982962677686266711E-15 ) ) ;
#1108 =( NAMED_UNIT ( * ) SI_UNIT ( $, .STERADIAN. ) SOLID_ANGLE_UNIT ( ) );
#1110 = EDGE_LOOP ( 'NONE', ( #18474, #16376, #16374, #13922 ) ) ;
#1109 = ORIENTED_EDGE ( 'NONE', *, *, #19459, .F. ) ;
#1111 = AXIS2_PLACEMENT_3D ( 'NONE', #3066, #8523, #15764 ) ;
#1112 = DIRECTION ( 'NONE',  ( -0.9873505073845697533, -0.1585527532634883330, -5.551115123125782702E-17 ) ) ;
#1114 = VECTOR ( 'NONE', #12180, 1000.000000000000000 ) ;
#1113 = STYLED_ITEM ( 'NONE', ( #18904 ), #6409 ) ;
#1116 = CARTESIAN_POINT ( 'NONE',  ( 7.500000000000000000, -4.730916290271713898, -7.493595886788494198 ) ) ;
#1115 = VECTOR ( 'NONE', #10599, 1000.000000000000000 ) ;
#1117 = CARTESIAN_POINT ( 'NONE',  ( 35.00000000000000711, 0.000000000000000000, -177.2000000000013529 ) ) ;
#1118 = TOROIDAL_SURFACE ( 'NONE', #6977, 5.384454397937118664, 0.5155456020628804703 ) ;
#1119 = AXIS2_PLACEMENT_3D ( 'NONE', #5628, #14944, #12816 ) ;
#1120 = CIRCLE ( 'NONE', #22717, 4.000000000000000000 ) ;
#1121 = AXIS2_PLACEMENT_3D ( 'NONE', #4909, #12668, #14115 ) ;
#1122 = DIRECTION ( 'NONE',  ( 0.000000000000000000, 0.000000000000000000, -1.000000000000000000 ) ) ;
#1123 = DIRECTION ( 'NONE',  ( -0.000000000000000000, 1.000000000000000000, -4.183096374613631247E-18 ) ) ;
#1124 = CARTESIAN_POINT ( 'NONE',  ( -285.0646579186753797, 269.1610889986682196, -146.2440776823445390 ) ) ;
#1125 = ORIENTED_EDGE ( 'NONE', *, *, #353, .F. ) ;
#1126 = DIRECTION ( 'NONE',  ( 0.000000000000000000, 0.000000000000000000, 1.000000000000000000 ) ) ;
#1127 = VERTEX_POINT ( 'NONE', #1331 ) ;
#1128 = DIRECTION ( 'NONE',  ( -0.000000000000000000, 0.000000000000000000, -1.000000000000000000 ) ) ;
#1129 = PLANE ( 'NONE',  #19628 ) ;
#1130 = ADVANCED_FACE ( 'NONE', ( #17882 ), #23560, .F. ) ;
#1131 = VERTEX_POINT ( 'NONE', #6538 ) ;
#1132 = CARTESIAN_POINT ( 'NONE',  ( 52.00000000000000711, -56.80000000000001137, 2.055021403285668792E-13 ) ) ;
#1133 = ORIENTED_EDGE ( 'NONE', *, *, #9813, .T. ) ;
#1134 = LINE ( 'NONE', #11809, #5012 ) ;
#1135 = FACE_OUTER_BOUND ( 'NONE', #14500, .T. ) ;
#1136 = AXIS2_PLACEMENT_3D ( 'NONE', #15984, #23328, #3275 ) ;
#1137 = ORIENTED_EDGE ( 'NONE', *, *, #6971, .F. ) ;
#1138 = LINE ( 'NONE', #23699, #20177 ) ;
#1139 = AXIS2_PLACEMENT_3D ( 'NONE', #8048, #21315, #12297 ) ;
#1140 = AXIS2_PLACEMENT_3D ( 'NONE', #651, #11317, #18625 ) ;
#1141 = CARTESIAN_POINT ( 'NONE',  ( 144.8060344827585482, 7.497491405673236464, -90.00000000000000000 ) ) ;
#1142 = CIRCLE ( 'NONE', #20035, 2.649999999999999467 ) ;
#1143 = VECTOR ( 'NONE', #17947, 1000.000000000000000 ) ;
#1144 = DIRECTION ( 'NONE',  ( 1.000000000000000000, 0.000000000000000000, 0.000000000000000000 ) ) ;
#1145 = EDGE_CURVE ( 'NONE', #20782, #4317, #9888, .T. ) ;
#1146 = FACE_OUTER_BOUND ( 'NONE', #5619, .T. ) ;
#1147 = CARTESIAN_POINT ( 'NONE',  ( 280.9755403010747159, 269.7771302778489826, 145.4357197208657340 ) ) ;
#1148 = VECTOR ( 'NONE', #21385, 1000.000000000000000 ) ;
#1149 = DIRECTION ( 'NONE',  ( -0.000000000000000000, -0.000000000000000000, 1.000000000000000000 ) ) ;
#1150 = EDGE_CURVE ( 'NONE', #7557, #1864, #19432, .T. ) ;
#1151 = CARTESIAN_POINT ( 'NONE',  ( -20.63749999999999574, 2.936090700955779752E-15, 23.97500000000000497 ) ) ;
#1152 = EDGE_LOOP ( 'NONE', ( #4727, #12791 ) ) ;
#1153 = DIRECTION ( 'NONE',  ( 0.000000000000000000, 0.000000000000000000, 1.000000000000000000 ) ) ;
#1154 = DIRECTION ( 'NONE',  ( 1.000000000000000000, 0.000000000000000000, 0.000000000000000000 ) ) ;
#1155 = ADVANCED_FACE ( 'NONE', ( #19690 ), #10664, .F. ) ;
#1156 = VERTEX_POINT ( 'NONE', #21271 ) ;
#1157 = VERTEX_POINT ( 'NONE', #15962 ) ;
#1158 = DIRECTION ( 'NONE',  ( 0.000000000000000000, 0.000000000000000000, -1.000000000000000000 ) ) ;
#1159 = DIRECTION ( 'NONE',  ( -0.000000000000000000, 1.103561164596346103E-15, 1.000000000000000000 ) ) ;
#1160 = PRODUCT_DEFINITION_FORMATION_WITH_SPECIFIED_SOURCE ( 'ANY', '', #23269, .NOT_KNOWN. ) ;
#1161 = STYLED_ITEM ( 'NONE', ( #8363 ), #19351 ) ;
#1162 = CIRCLE ( 'NONE', #12782, 2.199999999999979750 ) ;
#1163 = CONICAL_SURFACE ( 'NONE', #10852, 5.000000000000001776, 0.9599310885968795892 ) ;
#1164 = CARTESIAN_POINT ( 'NONE',  ( -281.4928932188135491, -132.2000000000000455, 150.2000000000013813 ) ) ;
#1165 = AXIS2_PLACEMENT_3D ( 'NONE', #13877, #15664, #1154 ) ;
#1166 = LINE ( 'NONE', #810, #15749 ) ;
#1167 = CARTESIAN_POINT ( 'NONE',  ( -283.7968359015655437, 271.3570580646226631, -145.7774350431394907 ) ) ;
#1168 = LINE ( 'NONE', #10860, #8480 ) ;
#1169 = ORIENTED_EDGE ( 'NONE', *, *, #6665, .F. ) ;
#1170 = DIRECTION ( 'NONE',  ( -3.469446951953613696E-16, 1.000000000000000000, 0.000000000000000000 ) ) ;
#1171 = CARTESIAN_POINT ( 'NONE',  ( 90.00000000000000000, 2.914335439641035919E-13, 129.9038105676659711 ) ) ;
#1172 = SURFACE_STYLE_FILL_AREA ( #22793 ) ;
#1173 = EDGE_LOOP ( 'NONE', ( #15595, #19148, #21434, #576 ) ) ;
#1174 = DIRECTION ( 'NONE',  ( 0.000000000000000000, 0.000000000000000000, 1.000000000000000000 ) ) ;
#1175 = ADVANCED_FACE ( 'NONE', ( #23193 ), #14559, .F. ) ;
#1176 = DIRECTION ( 'NONE',  ( 4.183096374613631247E-18, -1.000000000000000000, 0.000000000000000000 ) ) ;
#1177 = CARTESIAN_POINT ( 'NONE',  ( 50.00000000000000000, 0.000000000000000000, 3.000000000000000000 ) ) ;
#1178 = APPLICATION_PROTOCOL_DEFINITION ( 'draft international standard', 'automotive_design', 1998, #17104 ) ;
#1179 = CYLINDRICAL_SURFACE ( 'NONE', #16892, 5.249999999999973355 ) ;
#1180 = CARTESIAN_POINT ( 'NONE',  ( 65.00000000000001421, -52.79999999999938609, 125.0000000000002274 ) ) ;
#1181 = DIRECTION ( 'NONE',  ( -1.000000000000000000, 0.000000000000000000, 0.000000000000000000 ) ) ;
#1182 = VECTOR ( 'NONE', #15686, 1000.000000000000000 ) ;
#1183 = VECTOR ( 'NONE', #18740, 1000.000000000000000 ) ;
#1184 = ORIENTED_EDGE ( 'NONE', *, *, #3190, .F. ) ;
#1185 = ORIENTED_EDGE ( 'NONE', *, *, #3808, .F. ) ;
#1186 = CARTESIAN_POINT ( 'NONE',  ( -281.2431816561011715, 268.3724317483737423, -147.1290760626066856 ) ) ;
#1187 = CARTESIAN_POINT ( 'NONE',  ( 67.35000000000002274, -87.33333333333332860, 124.9999999999999858 ) ) ;
#1188 = EDGE_CURVE ( 'NONE', #12219, #19824, #2031, .T. ) ;
#1189 = ORIENTED_EDGE ( 'NONE', *, *, #22007, .T. ) ;
#1190 = EDGE_CURVE ( 'NONE', #13805, #10145, #18337, .T. ) ;
#1191 = CARTESIAN_POINT ( 'NONE',  ( 0.2500000000000002220, 0.000000000000000000, 0.000000000000000000 ) ) ;
#1192 = PLANE ( 'NONE',  #21511 ) ;
#1193 = ORIENTED_EDGE ( 'NONE', *, *, #16139, .F. ) ;
#1194 = DIRECTION ( 'NONE',  ( 0.000000000000000000, -0.4999999999999992228, 0.8660254037844390407 ) ) ;
#1195 = EDGE_CURVE ( 'NONE', #19464, #19646, #9096, .T. ) ;
#1196 = CARTESIAN_POINT ( 'NONE',  ( 1.206569728928466700, 7.963640680051486953, -0.4524126574264497602 ) ) ;
#1197 = ORIENTED_EDGE ( 'NONE', *, *, #5452, .T. ) ;
#1198 = LINE ( 'NONE', #13923, #16019 ) ;
#1199 = EDGE_CURVE ( 'NONE', #21582, #14233, #11844, .T. ) ;
#1200 = ORIENTED_EDGE ( 'NONE', *, *, #4425, .F. ) ;
#1201 = CARTESIAN_POINT ( 'NONE',  ( -44.99999999999995026, -52.79999999999969162, 52.65000000000017621 ) ) ;
#1202 = DIRECTION ( 'NONE',  ( 1.000000000000000000, 0.000000000000000000, 0.000000000000000000 ) ) ;
#1203 = ORIENTED_EDGE ( 'NONE', *, *, #19391, .F. ) ;
#1204 = ORIENTED_EDGE ( 'NONE', *, *, #18714, .T. ) ;
#1205 = CARTESIAN_POINT ( 'NONE',  ( 133.2566323304059495, 79.16876461166333456, -32.37389708099360774 ) ) ;
#1206 = PRODUCT_DEFINITION_SHAPE ( 'NONE', 'NONE',  #23832 ) ;
#1207 = DIRECTION ( 'NONE',  ( 1.221966984364620947E-29, 3.495664435217746987E-15, -1.000000000000000000 ) ) ;
#1208 = CARTESIAN_POINT ( 'NONE',  ( 2.500000000000002220, 0.000000000000000000, 0.000000000000000000 ) ) ;
#1209 = CARTESIAN_POINT ( 'NONE',  ( -2.558993250147282073, 7.638875775587784744, -7.593821156097241065 ) ) ;
#1210 = DIRECTION ( 'NONE',  ( -0.000000000000000000, -0.000000000000000000, 1.000000000000000000 ) ) ;
#1211 = ORIENTED_EDGE ( 'NONE', *, *, #5766, .T. ) ;
#1212 = EDGE_CURVE ( 'NONE', #11269, #931, #16668, .T. ) ;
#1213 = DIRECTION ( 'NONE',  ( -0.000000000000000000, 7.709882115452476934E-17, -1.000000000000000000 ) ) ;
#1214 = ORIENTED_EDGE ( 'NONE', *, *, #15943, .F. ) ;
#1215 = EDGE_CURVE ( 'NONE', #10931, #3015, #16546, .T. ) ;
#1216 = VERTEX_POINT ( 'NONE', #21849 ) ;
#1217 = CARTESIAN_POINT ( 'NONE',  ( 110.0000000000000000, -74.99999999999998579, 0.000000000000000000 ) ) ;
#1218 = ADVANCED_FACE ( 'NONE', ( #7472 ), #7018, .T. ) ;
#1219 = VERTEX_POINT ( 'NONE', #12614 ) ;
#1221 = EDGE_CURVE ( 'NONE', #21906, #11842, #4475, .T. ) ;
#1220 = CARTESIAN_POINT ( 'NONE',  ( 5.147825380264231754, 5.688155668806028409, -7.450218641347809090 ) ) ;
#1222 = ORIENTED_EDGE ( 'NONE', *, *, #5330, .T. ) ;
#1223 = CARTESIAN_POINT ( 'NONE',  ( -136.9835704417550915, -1072.529321614197215, 30.32918505548582644 ) ) ;
#1224 = ORIENTED_EDGE ( 'NONE', *, *, #9825, .T. ) ;
#1225 = CARTESIAN_POINT ( 'NONE',  ( 80.00000000000000000, -59.79999999999999005, 3.000000000000000000 ) ) ;
#1226 = CARTESIAN_POINT ( 'NONE',  ( 0.000000000000000000, 5.173457871231059415E-13, -150.2000000000008981 ) ) ;
#1227 = FACE_OUTER_BOUND ( 'NONE', #1740, .T. ) ;
#1228 = DIRECTION ( 'NONE',  ( -0.000000000000000000, -0.000000000000000000, -1.000000000000000000 ) ) ;
#1229 = CARTESIAN_POINT ( 'NONE',  ( 117.3074641843682144, -85.22886158240748955, -90.00000000000000000 ) ) ;
#1230 = ORIENTED_EDGE ( 'NONE', *, *, #6445, .T. ) ;
#1231 = DIRECTION ( 'NONE',  ( -0.9423651898111408132, -0.3345860861306287348, 6.982962677686266711E-15 ) ) ;
#1232 =( REPRESENTATION_RELATIONSHIP ('NONE','NONE', #10127, #5587 ) REPRESENTATION_RELATIONSHIP_WITH_TRANSFORMATION ( #407 )SHAPE_REPRESENTATION_RELATIONSHIP( ) );
#1234 = ORIENTED_EDGE ( 'NONE', *, *, #20465, .F. ) ;
#1233 = ORIENTED_EDGE ( 'NONE', *, *, #18027, .F. ) ;
#1235 = EDGE_CURVE ( 'NONE', #9811, #1621, #11604, .T. ) ;
#1236 = DIRECTION ( 'NONE',  ( 6.982962677686266711E-15, 0.000000000000000000, -1.000000000000000000 ) ) ;
#1237 = CARTESIAN_POINT ( 'NONE',  ( -1.250000000000000444, 7.938566201357357244, -7.198902722707429369 ) ) ;
#1238 = DIRECTION ( 'NONE',  ( -0.000000000000000000, 0.000000000000000000, 1.000000000000000000 ) ) ;
#1239 = DIRECTION ( 'NONE',  ( 0.000000000000000000, 2.618450529776326854E-15, 1.000000000000000000 ) ) ;
#1240 = CARTESIAN_POINT ( 'NONE',  ( 0.000000000000000000, 0.000000000000000000, 0.000000000000000000 ) ) ;
#1241 = DIRECTION ( 'NONE',  ( -0.000000000000000000, -0.000000000000000000, -1.000000000000000000 ) ) ;
#1242 = ADVANCED_FACE ( 'NONE', ( #18343 ), #9189, .F. ) ;
#1243 = ORIENTED_EDGE ( 'NONE', *, *, #1911, .T. ) ;
#1244 = EDGE_CURVE ( 'NONE', #12407, #10771, #17975, .T. ) ;
#1245 = DIRECTION ( 'NONE',  ( 3.736327486719275871E-16, -1.000000000000000000, 3.469446951953613794E-15 ) ) ;
#1246 = EDGE_CURVE ( 'NONE', #8826, #18148, #21051, .T. ) ;
#1247 = VERTEX_POINT ( 'NONE', #14867 ) ;
#1248 = CARTESIAN_POINT ( 'NONE',  ( 145.9999999999998010, -207.9449999999996805, 30.00000000000641620 ) ) ;
#1249 = LINE ( 'NONE', #12167, #2291 ) ;
#1250 = ITEM_DEFINED_TRANSFORMATION ( 'NONE', 'NONE', #19647,  #11210 ) ;
#1251 = ORIENTED_EDGE ( 'NONE', *, *, #2208, .F. ) ;
#1252 = AXIS2_PLACEMENT_3D ( 'NONE', #4431, #462, #11840 ) ;
#1253 = CARTESIAN_POINT ( 'NONE',  ( -3.472371940586054251, -2.614027278893156669, -3.320322319202162031 ) ) ;
#1254 = ORIENTED_EDGE ( 'NONE', *, *, #16181, .T. ) ;
#1255 = CARTESIAN_POINT ( 'NONE',  ( 155.0000000000000284, 2.775557561562891351E-16, 90.00000000000000000 ) ) ;
#1256 = CARTESIAN_POINT ( 'NONE',  ( 0.000000000000000000, 0.000000000000000000, -90.00000000000000000 ) ) ;
#1257 = VERTEX_POINT ( 'NONE', #22201 ) ;
#1258 = LINE ( 'NONE', #23228, #15953 ) ;
#1259 = FACE_OUTER_BOUND ( 'NONE', #10230, .T. ) ;
#1260 = LINE ( 'NONE', #1491, #9578 ) ;
#1261 = CARTESIAN_POINT ( 'NONE',  ( 4.211140560182196957, -2.431303136016555122, -3.745885042887436622 ) ) ;
#1262 = CARTESIAN_POINT ( 'NONE',  ( 90.00000000000000000, 2.914335439641035919E-13, 129.9038105676659711 ) ) ;
#1263 = FACE_OUTER_BOUND ( 'NONE', #6850, .T. ) ;
#1264 = CARTESIAN_POINT ( 'NONE',  ( 0.000000000000000000, 5.051668046482832750E-16, -4.000000000000000000 ) ) ;
#1265 = ORIENTED_EDGE ( 'NONE', *, *, #3366, .F. ) ;
#1266 = CARTESIAN_POINT ( 'NONE',  ( -79.99999999999995737, -62.00000000000004263, 0.000000000000000000 ) ) ;
#1267 = CARTESIAN_POINT ( 'NONE',  ( 0.000000000000000000, 0.000000000000000000, -90.00000000000000000 ) ) ;
#1268 = VERTEX_POINT ( 'NONE', #5671 ) ;
#1269 = EDGE_LOOP ( 'NONE', ( #15243, #18785, #1846, #6416 ) ) ;
#1270 = CARTESIAN_POINT ( 'NONE',  ( 1.500000000000000000, 0.000000000000000000, 0.000000000000000000 ) ) ;
#1271 = LINE ( 'NONE', #910, #18058 ) ;
#1272 = DIRECTION ( 'NONE',  ( -0.000000000000000000, 1.000000000000000000, 0.000000000000000000 ) ) ;
#1273 = FACE_OUTER_BOUND ( 'NONE', #8704, .T. ) ;
#1274 = CARTESIAN_POINT ( 'NONE',  ( -284.2295083325149108, 270.8299054689546779, -145.9020829022173871 ) ) ;
#1275 = ORIENTED_EDGE ( 'NONE', *, *, #157, .T. ) ;
#1276 = DIRECTION ( 'NONE',  ( 0.000000000000000000, 0.000000000000000000, -1.000000000000000000 ) ) ;
#1277 = VERTEX_POINT ( 'NONE', #3856 ) ;
#1278 = CARTESIAN_POINT ( 'NONE',  ( 0.000000000000000000, 0.000000000000000000, -90.00000000000000000 ) ) ;
#1279 = CARTESIAN_POINT ( 'NONE',  ( 45.24999999999994316, 100.0000000000000000, 150.2000000000009550 ) ) ;
#1280 = VECTOR ( 'NONE', #12258, 1000.000000000000000 ) ;
#1281 = DIRECTION ( 'NONE',  ( -0.000000000000000000, -0.000000000000000000, 1.000000000000000000 ) ) ;
#1282 = ORIENTED_EDGE ( 'NONE', *, *, #18033, .T. ) ;
#1283 = CARTESIAN_POINT ( 'NONE',  ( 4.000000000000000000, -1.084202172485504434E-14, -3.142992957459231906 ) ) ;
#1284 = VECTOR ( 'NONE', #5986, 1000.000000000000000 ) ;
#1285 = CARTESIAN_POINT ( 'NONE',  ( 281.4928932188133786, -129.2000000000000455, 177.2000000000014097 ) ) ;
#1286 = CARTESIAN_POINT ( 'NONE',  ( 105.0000000000000000, 35.00000000000000000, 0.000000000000000000 ) ) ;
#1287 = DIRECTION ( 'NONE',  ( 0.000000000000000000, 0.000000000000000000, -1.000000000000000000 ) ) ;
#1288 = CARTESIAN_POINT ( 'NONE',  ( -20.00000000000000000, 2.449293598294706513E-15, -125.0000000000000000 ) ) ;
#1289 = DIRECTION ( 'NONE',  ( 4.183096374613631247E-18, 1.000000000000000000, 0.000000000000000000 ) ) ;
#1290 = DIRECTION ( 'NONE',  ( 0.000000000000000000, 0.000000000000000000, -1.000000000000000000 ) ) ;
#1291 = ORIENTED_EDGE ( 'NONE', *, *, #17411, .F. ) ;
#1292 = ORIENTED_EDGE ( 'NONE', *, *, #17778, .T. ) ;
#1293 = LINE ( 'NONE', #1412, #19171 ) ;
#1294 = CARTESIAN_POINT ( 'NONE',  ( -20.00000000000000000, -1000.000000000000000, 124.9999999999998579 ) ) ;
#1295 = VERTEX_POINT ( 'NONE', #11268 ) ;
#1296 = VECTOR ( 'NONE', #8454, 1000.000000000000000 ) ;
#1297 = DIRECTION ( 'NONE',  ( -1.000000000000000000, -0.000000000000000000, -0.000000000000000000 ) ) ;
#1299 = CIRCLE ( 'NONE', #4783, 2.499999999999998668 ) ;
#1298 = CARTESIAN_POINT ( 'NONE',  ( 2.500000000000000000, 2.500728763858895382E-16, -2.041999999999999815 ) ) ;
#1300 = ADVANCED_FACE ( 'NONE', ( #18575 ), #14405, .F. ) ;
#1301 = VERTEX_POINT ( 'NONE', #22323 ) ;
#1302 = DIRECTION ( 'NONE',  ( 0.000000000000000000, 0.000000000000000000, -1.000000000000000000 ) ) ;
#1303 = ADVANCED_FACE ( 'NONE', ( #4461 ), #20888, .F. ) ;
#1304 = FACE_OUTER_BOUND ( 'NONE', #3498, .T. ) ;
#1305 = ORIENTED_EDGE ( 'NONE', *, *, #23640, .T. ) ;
#1306 = PLANE ( 'NONE',  #17938 ) ;
#1307 = EDGE_CURVE ( 'NONE', #12981, #9371, #16811, .T. ) ;
#1308 = ORIENTED_EDGE ( 'NONE', *, *, #15523, .F. ) ;
#1309 = DIRECTION ( 'NONE',  ( 1.000000000000000000, 0.000000000000000000, 0.000000000000000000 ) ) ;
#1310 = EDGE_CURVE ( 'NONE', #644, #18250, #10269, .T. ) ;
#1311 = ADVANCED_FACE ( 'NONE', ( #20749 ), #18810, .F. ) ;
#1312 = DIRECTION ( 'NONE',  ( 0.000000000000000000, 0.000000000000000000, 1.000000000000000000 ) ) ;
#1313 = ORIENTED_EDGE ( 'NONE', *, *, #647, .F. ) ;
#1314 = VERTEX_POINT ( 'NONE', #2400 ) ;
#1315 = CYLINDRICAL_SURFACE ( 'NONE', #4216, 2.649999999999999467 ) ;
#1316 = CARTESIAN_POINT ( 'NONE',  ( -91.18044947428876412, -112.7436279071535239, -90.00000000000000000 ) ) ;
#1317 = CIRCLE ( 'NONE', #7476, 7.499999999999996447 ) ;
#1318 = CARTESIAN_POINT ( 'NONE',  ( 0.3470952277635277472, 8.860649561028097310, -7.493596212620242447 ) ) ;
#1319 = AXIS2_PLACEMENT_3D ( 'NONE', #708, #4337, #364 ) ;
#1320 = CARTESIAN_POINT ( 'NONE',  ( -312.2000000000014666, -132.2000000000000455, -146.4928932188134070 ) ) ;
#1321 = EDGE_CURVE ( 'NONE', #13384, #21062, #15345, .T. ) ;
#1322 = VERTEX_POINT ( 'NONE', #17268 ) ;
#1323 = DIRECTION ( 'NONE',  ( -0.000000000000000000, -0.000000000000000000, 1.000000000000000000 ) ) ;
#1324 = ORIENTED_EDGE ( 'NONE', *, *, #4746, .T. ) ;
#1325 = VECTOR ( 'NONE', #16725, 999.9999999999997726 ) ;
#1326 = DIRECTION ( 'NONE',  ( 0.000000000000000000, 1.177509268541832635E-16, -1.000000000000000000 ) ) ;
#1327 = VECTOR ( 'NONE', #3793, 1000.000000000000114 ) ;
#1328 = DIRECTION ( 'NONE',  ( 0.000000000000000000, 0.000000000000000000, -1.000000000000000000 ) ) ;
#1329 = AXIS2_PLACEMENT_3D ( 'NONE', #9733, #11807, #22623 ) ;
#1330 = ORIENTED_EDGE ( 'NONE', *, *, #4417, .T. ) ;
#1331 = CARTESIAN_POINT ( 'NONE',  ( 0.2500000000000002220, 5.204748896376250699E-16, -4.250000000000000000 ) ) ;
#1332 = VECTOR ( 'NONE', #19926, 1000.000000000000000 ) ;
#1333 = CIRCLE ( 'NONE', #952, 145.0000000000000284 ) ;
#1334 = EDGE_LOOP ( 'NONE', ( #13815, #13963, #11908, #18201, #9704 ) ) ;
#1335 = FACE_OUTER_BOUND ( 'NONE', #15483, .T. ) ;
#1336 = EDGE_CURVE ( 'NONE', #3845, #2034, #5803, .T. ) ;
#1337 = ORIENTED_EDGE ( 'NONE', *, *, #20218, .T. ) ;
#1338 = ADVANCED_FACE ( 'NONE', ( #11373 ), #22809, .T. ) ;
#1339 = CYLINDRICAL_SURFACE ( 'NONE', #13540, 24.99999999999998224 ) ;
#1340 = EDGE_CURVE ( 'NONE', #2213, #6626, #7845, .T. ) ;
#1341 = CARTESIAN_POINT ( 'NONE',  ( 7.500000000000000000, -4.330127018922199866, -7.422398894150035176 ) ) ;
#1342 = DIRECTION ( 'NONE',  ( 1.000000000000000000, -6.938893903907227392E-16, 0.000000000000000000 ) ) ;
#1343 = DIRECTION ( 'NONE',  ( 0.000000000000000000, 0.000000000000000000, -1.000000000000000000 ) ) ;
#1344 = EDGE_CURVE ( 'NONE', #18619, #4703, #7733, .T. ) ;
#1345 = TOROIDAL_SURFACE ( 'NONE', #8046, 22.50000000000000000, 1.500000000000000444 ) ;
#1346 = EDGE_CURVE ( 'NONE', #19016, #7096, #712, .T. ) ;
#1347 = DIRECTION ( 'NONE',  ( 0.000000000000000000, 1.000000000000000000, -5.286776307738891306E-15 ) ) ;
#1348 = EDGE_LOOP ( 'NONE', ( #12123, #14832, #17782, #8128, #19299, #19905, #4504, #17414, #12961, #17013, #23561, #6301 ) ) ;
#1349 = LINE ( 'NONE', #17789, #15417 ) ;
#1350 = EDGE_CURVE ( 'NONE', #9824, #17073, #13684, .T. ) ;
#1351 = AXIS2_PLACEMENT_3D ( 'NONE', #11749, #715, #6029 ) ;
#1353 = EDGE_LOOP ( 'NONE', ( #21943, #75 ) ) ;
#1352 = VERTEX_POINT ( 'NONE', #2279 ) ;
#1354 = DIRECTION ( 'NONE',  ( 2.832769448823989808E-16, -1.000000000000000000, 3.469446951953613794E-15 ) ) ;
#1355 = CARTESIAN_POINT ( 'NONE',  ( 0.000000000000000000, -1.178949249685214307, 2.042000000000001592 ) ) ;
#1356 = CARTESIAN_POINT ( 'NONE',  ( -288.2000000000006708, 90.00000000000100897, 34.99999999999999289 ) ) ;
#1357 = DIRECTION ( 'NONE',  ( -1.000000000000000000, 0.000000000000000000, 0.000000000000000000 ) ) ;
#1358 = DIRECTION ( 'NONE',  ( -1.000000000000000000, 7.709882115452476934E-17, 0.000000000000000000 ) ) ;
#1359 = CIRCLE ( 'NONE', #4052, 5.199999999999982414 ) ;
#1360 = ORIENTED_EDGE ( 'NONE', *, *, #12442, .T. ) ;
#1361 = CARTESIAN_POINT ( 'NONE',  ( 7.500000000000000000, -3.988190556646209028, -0.8526458641284331286 ) ) ;
#1362 = ORIENTED_EDGE ( 'NONE', *, *, #22126, .F. ) ;
#1363 = FACE_OUTER_BOUND ( 'NONE', #12024, .T. ) ;
#1364 = DIRECTION ( 'NONE',  ( 0.000000000000000000, 0.000000000000000000, -1.000000000000000000 ) ) ;
#1365 = ITEM_DEFINED_TRANSFORMATION ( 'NONE', 'NONE', #774,  #11210 ) ;
#1366 = EDGE_LOOP ( 'NONE', ( #4331, #2748, #2855, #13215 ) ) ;
#1367 = VECTOR ( 'NONE', #17921, 1000.000000000000000 ) ;
#1368 = CARTESIAN_POINT ( 'NONE',  ( -44.80746418436648071, -137.9031948627975908, -90.00000000000000000 ) ) ;
#1369 = ORIENTED_EDGE ( 'NONE', *, *, #15166, .T. ) ;
#1370 = CARTESIAN_POINT ( 'NONE',  ( 282.1999999999999318, 267.7999999999999545, 146.4928932188134922 ) ) ;
#1371 = DIRECTION ( 'NONE',  ( 0.000000000000000000, 0.000000000000000000, -1.000000000000000000 ) ) ;
#1372 = EDGE_LOOP ( 'NONE', ( #10743, #20653, #3624, #2809 ) ) ;
#1373 = CARTESIAN_POINT ( 'NONE',  ( 133.9567665909156915, 77.97815834559359871, 31.25900233431400110 ) ) ;
#1374 = CARTESIAN_POINT ( 'NONE',  ( 45.00000000000002132, -52.79999999999934346, 195.0000000000002274 ) ) ;
#1375 = DIRECTION ( 'NONE',  ( 0.000000000000000000, 0.000000000000000000, -1.000000000000000000 ) ) ;
#1376 = ADVANCED_FACE ( 'NONE', ( #19177 ), #11869, .T. ) ;
#1377 = CARTESIAN_POINT ( 'NONE',  ( 2.700000000000001510, 3.024877593893962577E-15, 24.69999999999999929 ) ) ;
#1378 = VECTOR ( 'NONE', #2350, 1000.000000000000000 ) ;
#1379 = ADVANCED_FACE ( 'NONE', ( #11635 ), #2640, .F. ) ;
#1380 = CARTESIAN_POINT ( 'NONE',  ( -31.74999999999994316, 5.204748896376250699E-16, -4.250000000000000000 ) ) ;
#1381 = DIRECTION ( 'NONE',  ( -1.000000000000000000, 0.000000000000000000, -0.000000000000000000 ) ) ;
#1382 = EDGE_LOOP ( 'NONE', ( #20054, #9582 ) ) ;
#1383 = VECTOR ( 'NONE', #18125, 1000.000000000000000 ) ;
#1384 = SURFACE_SIDE_STYLE ('',( #14555 ) ) ;
#1385 = FACE_OUTER_BOUND ( 'NONE', #21095, .T. ) ;
#1386 = CARTESIAN_POINT ( 'NONE',  ( 3.749999999999999112, -6.495190528383302464, -6.991905250253757309 ) ) ;
#1387 = AXIS2_PLACEMENT_3D ( 'NONE', #13984, #21307, #4758 ) ;
#1388 = ORIENTED_EDGE ( 'NONE', *, *, #20616, .F. ) ;
#1389 = DIRECTION ( 'NONE',  ( 0.5877852522924826850, -0.8090169943749405679, 0.000000000000000000 ) ) ;
#1390 = DIRECTION ( 'NONE',  ( 0.000000000000000000, 1.177509268541832635E-16, -1.000000000000000000 ) ) ;
#1392 = CARTESIAN_POINT ( 'NONE',  ( 7.499999999999999112, 41.99999999999998579, -100.0000000000000000 ) ) ;
#1391 = PRODUCT_DEFINITION_SHAPE ( 'NONE', 'NONE',  #23820 ) ;
#1393 = VECTOR ( 'NONE', #20319, 1000.000000000000000 ) ;
#1394 = DIRECTION ( 'NONE',  ( -0.000000000000000000, -0.000000000000000000, 1.000000000000000000 ) ) ;
#1395 = DIRECTION ( 'NONE',  ( 1.000000000000000000, -0.000000000000000000, -0.000000000000000000 ) ) ;
#1396 = EDGE_LOOP ( 'NONE', ( #13575, #10334, #6051, #16215 ) ) ;
#1397 = FACE_OUTER_BOUND ( 'NONE', #1757, .T. ) ;
#1398 = VERTEX_POINT ( 'NONE', #600 ) ;
#1399 = DIRECTION ( 'NONE',  ( -1.000000000000000000, 0.000000000000000000, 0.000000000000000000 ) ) ;
#1400 = CARTESIAN_POINT ( 'NONE',  ( 0.000000000000000000, 0.000000000000000000, -0.5251556536572846712 ) ) ;
#1401 = DIRECTION ( 'NONE',  ( -1.000000000000000000, -0.000000000000000000, -0.000000000000000000 ) ) ;
#1402 = ORIENTED_EDGE ( 'NONE', *, *, #2339, .F. ) ;
#1403 = DIRECTION ( 'NONE',  ( -0.000000000000000000, -1.177509268541832635E-16, 1.000000000000000000 ) ) ;
#1404 = FACE_OUTER_BOUND ( 'NONE', #16223, .T. ) ;
#1405 = LINE ( 'NONE', #21806, #15791 ) ;
#1406 = FACE_OUTER_BOUND ( 'NONE', #5182, .T. ) ;
#1407 = DIRECTION ( 'NONE',  ( 0.000000000000000000, 0.000000000000000000, -1.000000000000000000 ) ) ;
#1408 = CARTESIAN_POINT ( 'NONE',  ( 24.33333333333333215, -89.99999999999998579, 3.000000000000000000 ) ) ;
#1409 = CARTESIAN_POINT ( 'NONE',  ( 5.000000000000000888, 0.000000000000000000, 0.000000000000000000 ) ) ;
#1410 = ORIENTED_EDGE ( 'NONE', *, *, #16821, .T. ) ;
#1411 = ORIENTED_EDGE ( 'NONE', *, *, #22522, .F. ) ;
#1412 = CARTESIAN_POINT ( 'NONE',  ( -281.4928932188135491, -129.2000000000000455, 177.2000000000014097 ) ) ;
#1413 = AXIS2_PLACEMENT_3D ( 'NONE', #8127, #13816, #19200 ) ;
#1414 = CARTESIAN_POINT ( 'NONE',  ( 2.500000000000000000, -2.357898499370432610, 3.252606517456513302E-15 ) ) ;
#1415 = CARTESIAN_POINT ( 'NONE',  ( 284.1822575857424340, 271.0140793454687582, -145.8708543776411091 ) ) ;
#1416 = ORIENTED_EDGE ( 'NONE', *, *, #21211, .F. ) ;
#1417 = PLANE ( 'NONE',  #12387 ) ;
#1418 = DIRECTION ( 'NONE',  ( 0.000000000000000000, 0.000000000000000000, -1.000000000000000000 ) ) ;
#1419 = ORIENTED_EDGE ( 'NONE', *, *, #7745, .T. ) ;
#1420 = CARTESIAN_POINT ( 'NONE',  ( 155.0000000000000284, 2.775557561562891351E-16, 90.00000000000000000 ) ) ;
#1421 = FACE_OUTER_BOUND ( 'NONE', #4724, .T. ) ;
#1422 = ORIENTED_EDGE ( 'NONE', *, *, #898, .T. ) ;
#1423 = FACE_OUTER_BOUND ( 'NONE', #3117, .T. ) ;
#1424 = ORIENTED_EDGE ( 'NONE', *, *, #19677, .F. ) ;
#1425 = VECTOR ( 'NONE', #2146, 1000.000000000000000 ) ;
#1426 = CARTESIAN_POINT ( 'NONE',  ( 25.00000000000004263, -37.41657386773938754, 65.00000000000018474 ) ) ;
#1427 = DIRECTION ( 'NONE',  ( 0.000000000000000000, 0.000000000000000000, -1.000000000000000000 ) ) ;
#1428 = EDGE_LOOP ( 'NONE', ( #4910, #5715, #19219 ) ) ;
#1429 = ORIENTED_EDGE ( 'NONE', *, *, #12122, .F. ) ;
#1430 = EDGE_CURVE ( 'NONE', #14150, #10594, #202, .T. ) ;
#1431 = DIRECTION ( 'NONE',  ( -0.000000000000000000, 1.000000000000000000, -3.469446951953613794E-15 ) ) ;
#1432 = DIRECTION ( 'NONE',  ( 1.221966984364620947E-29, 3.495664435217746987E-15, -1.000000000000000000 ) ) ;
#1433 = DIRECTION ( 'NONE',  ( -0.000000000000000000, -1.000000000000000000, 0.000000000000000000 ) ) ;
#1434 = CARTESIAN_POINT ( 'NONE',  ( -145.0000000000000284, -1000.000000000000000, 90.00000000000000000 ) ) ;
#1435 = DIRECTION ( 'NONE',  ( 0.000000000000000000, 0.000000000000000000, 1.000000000000000000 ) ) ;
#1436 = ADVANCED_FACE ( 'NONE', ( #13210 ), #20510, .F. ) ;
#1437 = ORIENTED_EDGE ( 'NONE', *, *, #10670, .F. ) ;
#1438 = DIRECTION ( 'NONE',  ( 0.000000000000000000, 2.618450529776326854E-15, 1.000000000000000000 ) ) ;
#1439 = EDGE_CURVE ( 'NONE', #22213, #6889, #13436, .T. ) ;
#1440 = AXIS2_PLACEMENT_3D ( 'NONE', #204, #3567, #20000 ) ;
#1441 = ORIENTED_EDGE ( 'NONE', *, *, #20361, .T. ) ;
#1442 = AXIS2_PLACEMENT_3D ( 'NONE', #13504, #3692, #20685 ) ;
#1443 = EDGE_CURVE ( 'NONE', #4246, #14920, #21250, .T. ) ;
#1444 = AXIS2_PLACEMENT_3D ( 'NONE', #23645, #5648, #23539 ) ;
#1445 = CARTESIAN_POINT ( 'NONE',  ( 0.000000000000000000, -129.2000000000000455, -7.690461757479017101E-15 ) ) ;
#1446 = AXIS2_PLACEMENT_3D ( 'NONE', #145, #7865, #14889 ) ;
#1447 = FACE_OUTER_BOUND ( 'NONE', #2462, .T. ) ;
#1448 = ORIENTED_EDGE ( 'NONE', *, *, #7344, .T. ) ;
#1449 = CARTESIAN_POINT ( 'NONE',  ( 2.411464220263165092, 7.267994521134541586, -7.491772860716163329 ) ) ;
#1450 = ORIENTED_EDGE ( 'NONE', *, *, #2275, .F. ) ;
#1451 = FACE_OUTER_BOUND ( 'NONE', #6237, .T. ) ;
#1452 = VECTOR ( 'NONE', #1843, 1000.000000000000000 ) ;
#1453 = EDGE_LOOP ( 'NONE', ( #17995, #9504, #17274, #20589 ) ) ;
#1454 = DIRECTION ( 'NONE',  ( -1.000000000000000000, 0.000000000000000000, 0.000000000000000000 ) ) ;
#1455 = FILL_AREA_STYLE ('',( #4975 ) ) ;
#1456 = CIRCLE ( 'NONE', #13459, 160.0000000000000000 ) ;
#1457 = DIRECTION ( 'NONE',  ( 1.000000000000000000, 0.000000000000000000, -0.000000000000000000 ) ) ;
#1458 = CARTESIAN_POINT ( 'NONE',  ( -100.0000000000001137, -132.2000000000001592, 177.2000000000014097 ) ) ;
#1459 = AXIS2_PLACEMENT_3D ( 'NONE', #457, #15441, #6245 ) ;
#1460 = DIRECTION ( 'NONE',  ( 0.000000000000000000, -4.183096374613631247E-18, -1.000000000000000000 ) ) ;
#1461 = VERTEX_POINT ( 'NONE', #6864 ) ;
#1462 = CARTESIAN_POINT ( 'NONE',  ( 0.000000000000000000, 0.000000000000000000, 100.0000000000000000 ) ) ;
#1463 = SHAPE_REPRESENTATION_RELATIONSHIP ( 'NONE' , 'NONE' ,  #4684, #5256 ) ;
#1464 = EDGE_CURVE ( 'NONE', #10418, #3155, #14145, .T. ) ;
#1466 = ORIENTED_EDGE ( 'NONE', *, *, #21900, .T. ) ;
#1465 = EDGE_LOOP ( 'NONE', ( #6278, #20700, #142, #6382 ) ) ;
#1467 = DIRECTION ( 'NONE',  ( -0.6964005597823107463, 0.7176533009294141507, -6.982962677686266711E-15 ) ) ;
#1468 = CARTESIAN_POINT ( 'NONE',  ( 2.500000000000000000, 2.357898499370432166, -2.385244779468109755E-15 ) ) ;
#1469 = PLANE ( 'NONE',  #22255 ) ;
#1470 = EDGE_CURVE ( 'NONE', #19949, #13282, #5988, .T. ) ;
#1471 = CARTESIAN_POINT ( 'NONE',  ( -52.99999999999997158, 1.769673560495883054E-29, 4.723692975627390055E-15 ) ) ;
#1472 = EDGE_CURVE ( 'NONE', #15247, #5237, #1198, .T. ) ;
#1473 = CARTESIAN_POINT ( 'NONE',  ( -40.00000000000000000, 100.0000000000000000, 145.0000000000000000 ) ) ;
#1474 = CIRCLE ( 'NONE', #18053, 0.3000000000000051514 ) ;
#1475 = ORIENTED_EDGE ( 'NONE', *, *, #11144, .F. ) ;
#1476 = CIRCLE ( 'NONE', #6881, 2.649999999999985700 ) ;
#1477 = CARTESIAN_POINT ( 'NONE',  ( -31.74999999999995737, 3.061616997868383634E-16, -2.500000000000000444 ) ) ;
#1478 = AXIS2_PLACEMENT_3D ( 'NONE', #9714, #10185, #9952 ) ;
#1479 = EDGE_CURVE ( 'NONE', #8566, #22288, #7241, .T. ) ;
#1480 = ORIENTED_EDGE ( 'NONE', *, *, #116, .F. ) ;
#1481 = PRODUCT_RELATED_PRODUCT_CATEGORY ( 'part', '', ( #2824 ) ) ;
#1482 = DIRECTION ( 'NONE',  ( 0.000000000000000000, -0.7071067811865485719, -0.7071067811865465735 ) ) ;
#1483 = CARTESIAN_POINT ( 'NONE',  ( 2.500000000000000000, 0.000000000000000000, 0.000000000000000000 ) ) ;
#1484 = VECTOR ( 'NONE', #21691, 1000.000000000000000 ) ;
#1485 = ITEM_DEFINED_TRANSFORMATION ( 'NONE', 'NONE', #18877,  #11210 ) ;
#1486 = ORIENTED_EDGE ( 'NONE', *, *, #8980, .T. ) ;
#1487 = VERTEX_POINT ( 'NONE', #8213 ) ;
#1488 = CARTESIAN_POINT ( 'NONE',  ( 0.000000000000000000, 0.000000000000000000, 100.0000000000000000 ) ) ;
#1489 = ORIENTED_EDGE ( 'NONE', *, *, #11624, .T. ) ;
#1490 = DIRECTION ( 'NONE',  ( 0.000000000000000000, -1.000000000000000000, 0.000000000000000000 ) ) ;
#1491 = CARTESIAN_POINT ( 'NONE',  ( -31.74999999999994316, 0.000000000000000000, 4.250000000000000000 ) ) ;
#1492 = PRODUCT_DEFINITION_SHAPE ( 'NONE', 'NONE',  #21557 ) ;
#1493 = CARTESIAN_POINT ( 'NONE',  ( -7.499999999999999112, 34.18698582794336716, 100.0000000000000000 ) ) ;
#1495 = CIRCLE ( 'NONE', #1095, 2.499999999999998668 ) ;
#1494 = MECHANICAL_DESIGN_GEOMETRIC_PRESENTATION_REPRESENTATION (  '', ( #21614 ), #11168 ) ;
#1496 = CARTESIAN_POINT ( 'NONE',  ( -4.207491450040567571, 2.029819825146470524, -3.671670828759566074 ) ) ;
#1497 = CARTESIAN_POINT ( 'NONE',  ( -45.00000000000000000, 269.9999999999999432, -5.249999999999973355 ) ) ;
#1498 = AXIS2_PLACEMENT_3D ( 'NONE', #10621, #14371, #12334 ) ;
#1499 = AXIS2_PLACEMENT_3D ( 'NONE', #3288, #4753, #2922 ) ;
#1500 = VECTOR ( 'NONE', #17474, 1000.000000000000000 ) ;
#1501 = ORIENTED_EDGE ( 'NONE', *, *, #13204, .T. ) ;
#1502 = DIRECTION ( 'NONE',  ( -0.000000000000000000, -0.000000000000000000, 1.000000000000000000 ) ) ;
#1503 = DIRECTION ( 'NONE',  ( -6.486615240276975916E-15, -2.585650881802458380E-15, 1.000000000000000000 ) ) ;
#1504 = CIRCLE ( 'NONE', #2664, 5.249999999999949374 ) ;
#1505 = APPLICATION_CONTEXT ( 'automotive_design' ) ;
#1506 = VERTEX_POINT ( 'NONE', #1063 ) ;
#1507 = CARTESIAN_POINT ( 'NONE',  ( -281.4928932188134354, -129.2000000000000455, -152.4000000000012562 ) ) ;
#1508 = PLANE ( 'NONE',  #10688 ) ;
#1509 = LINE ( 'NONE', #3191, #4429 ) ;
#1510 = AXIS2_PLACEMENT_3D ( 'NONE', #7279, #14677, #17066 ) ;
#1511 = VECTOR ( 'NONE', #22387, 1000.000000000000114 ) ;
#1512 = EDGE_CURVE ( 'NONE', #16414, #21068, #17546, .T. ) ;
#1513 = CIRCLE ( 'NONE', #7691, 7.500000000000001776 ) ;
#1514 = CARTESIAN_POINT ( 'NONE',  ( 85.22886158240706322, 117.3074641843685129, -90.00000000000000000 ) ) ;
#1515 = AXIS2_PLACEMENT_3D ( 'NONE', #23513, #21696, #12679 ) ;
#1516 = EDGE_CURVE ( 'NONE', #9258, #16083, #23169, .T. ) ;
#1517 = DIRECTION ( 'NONE',  ( 0.000000000000000000, 0.000000000000000000, -1.000000000000000000 ) ) ;
#1518 = CIRCLE ( 'NONE', #16954, 7.499999999999998224 ) ;
#1519 = AXIS2_PLACEMENT_3D ( 'NONE', #4350, #20765, #2163 ) ;
#1520 = ORIENTED_EDGE ( 'NONE', *, *, #21180, .F. ) ;
#1521 = VECTOR ( 'NONE', #15755, 1000.000000000000000 ) ;
#1522 = AXIS2_PLACEMENT_3D ( 'NONE', #19276, #14003, #13890 ) ;
#1523 = CARTESIAN_POINT ( 'NONE',  ( 0.000000000000000000, 0.000000000000000000, 200.0000119999999981 ) ) ;
#1524 = VERTEX_POINT ( 'NONE', #12227 ) ;
#1525 = LINE ( 'NONE', #7427, #20637 ) ;
#1526 = CARTESIAN_POINT ( 'NONE',  ( 67.35000000000002274, -87.33333333333332860, 3.000000000000001332 ) ) ;
#1527 = SURFACE_STYLE_FILL_AREA ( #21581 ) ;
#1528 = VERTEX_POINT ( 'NONE', #10524 ) ;
#1529 = CARTESIAN_POINT ( 'NONE',  ( -4.406842699996122548, 6.115962218725288224, 1.165517335421917267E-15 ) ) ;
#1530 = CARTESIAN_POINT ( 'NONE',  ( 287.4000000000013415, -132.2000000000000455, 146.4928932188134638 ) ) ;
#1531 = CYLINDRICAL_SURFACE ( 'NONE', #372, 2.649999999999971934 ) ;
#1532 = FACE_BOUND ( 'NONE', #2193, .T. ) ;
#1533 = DIRECTION ( 'NONE',  ( 0.000000000000000000, 0.000000000000000000, 1.000000000000000000 ) ) ;
#1534 = CARTESIAN_POINT ( 'NONE',  ( -312.2000000000014666, -132.2000000000000455, 146.4928932188134638 ) ) ;
#1535 = CARTESIAN_POINT ( 'NONE',  ( 6.482064212728078090, 24.20041621714725721, 145.0000119999999697 ) ) ;
#1536 = ORIENTED_EDGE ( 'NONE', *, *, #16790, .F. ) ;
#1537 = ORIENTED_EDGE ( 'NONE', *, *, #7567, .T. ) ;
#1539 = AXIS2_PLACEMENT_3D ( 'NONE', #22452, #8220, #15597 ) ;
#1538 = AXIS2_PLACEMENT_3D ( 'NONE', #22491, #12050, #13841 ) ;
#1540 = FACE_OUTER_BOUND ( 'NONE', #15740, .T. ) ;
#1541 = DIRECTION ( 'NONE',  ( 0.000000000000000000, -0.000000000000000000, 1.000000000000000000 ) ) ;
#1542 = STYLED_ITEM ( 'NONE', ( #11425 ), #5256 ) ;
#1543 = VECTOR ( 'NONE', #23799, 1000.000000000000114 ) ;
#1544 = EDGE_LOOP ( 'NONE', ( #23507, #23295, #21687 ) ) ;
#1545 = AXIS2_PLACEMENT_3D ( 'NONE', #14639, #21749, #20056 ) ;
#1546 = AXIS2_PLACEMENT_3D ( 'NONE', #9149, #17967, #22161 ) ;
#1547 = DIRECTION ( 'NONE',  ( 0.8660254037844379305, 0.5000000000000013323, 0.000000000000000000 ) ) ;
#1548 = DIRECTION ( 'NONE',  ( 1.000000000000000000, 0.000000000000000000, 0.000000000000000000 ) ) ;
#1549 = ORIENTED_EDGE ( 'NONE', *, *, #14515, .T. ) ;
#1550 = CARTESIAN_POINT ( 'NONE',  ( 281.4928932188133217, 267.7999999999999545, 150.1999999999999886 ) ) ;
#1551 = AXIS2_PLACEMENT_3D ( 'NONE', #6724, #5046, #6611 ) ;
#1552 = DIRECTION ( 'NONE',  ( -0.000000000000000000, -0.000000000000000000, 1.000000000000000000 ) ) ;
#1553 = EDGE_LOOP ( 'NONE', ( #17397, #4963, #19044, #3864 ) ) ;
#1554 = EDGE_CURVE ( 'NONE', #23349, #12522, #2502, .T. ) ;
#1555 = FACE_BOUND ( 'NONE', #9941, .T. ) ;
#1556 = ORIENTED_EDGE ( 'NONE', *, *, #12045, .T. ) ;
#1557 = ADVANCED_FACE ( 'NONE', ( #22917 ), #1306, .F. ) ;
#1558 = DIRECTION ( 'NONE',  ( 0.000000000000000000, -1.110223024625156540E-16, 1.000000000000000000 ) ) ;
#1559 = DIRECTION ( 'NONE',  ( 1.000000000000000000, 0.000000000000000000, 0.000000000000000000 ) ) ;
#1561 = CONICAL_SURFACE ( 'NONE', #10003, 2.055000000000001492, 0.7853981633974633780 ) ;
#1560 = CARTESIAN_POINT ( 'NONE',  ( 126.3653543294818178, 77.28387428943173632, -32.05499999999358351 ) ) ;
#1562 = EDGE_LOOP ( 'NONE', ( #23282, #1362, #17315, #5755 ) ) ;
#1563 = ORIENTED_EDGE ( 'NONE', *, *, #18137, .T. ) ;
#1564 = CARTESIAN_POINT ( 'NONE',  ( 284.5436892194421148, 270.4188186979286002, -145.9952621458755857 ) ) ;
#1565 = CIRCLE ( 'NONE', #6182, 7.500000000000000888 ) ;
#1566 = AXIS2_PLACEMENT_3D ( 'NONE', #2201, #7778, #5721 ) ;
#1567 = DIRECTION ( 'NONE',  ( 1.000000000000000000, -3.495664435217746987E-15, 0.000000000000000000 ) ) ;
#1568 = LINE ( 'NONE', #17988, #14694 ) ;
#1569 = CARTESIAN_POINT ( 'NONE',  ( 0.2779000157839532359, 8.820699686765054892, -7.928862157988302961 ) ) ;
#1570 = DIRECTION ( 'NONE',  ( 1.000000000000000000, 0.000000000000000000, 0.000000000000000000 ) ) ;
#1571 = ORIENTED_EDGE ( 'NONE', *, *, #18407, .T. ) ;
#1572 = CARTESIAN_POINT ( 'NONE',  ( 6.482064212728086972, -24.20041621714725011, 145.0000119999999697 ) ) ;
#1573 = ORIENTED_EDGE ( 'NONE', *, *, #16696, .T. ) ;
#1574 = EDGE_CURVE ( 'NONE', #629, #10120, #22933, .T. ) ;
#1575 = DIRECTION ( 'NONE',  ( -0.000000000000000000, -0.000000000000000000, 1.000000000000000000 ) ) ;
#1576 = EDGE_CURVE ( 'NONE', #22418, #12831, #6749, .T. ) ;
#1577 = FACE_OUTER_BOUND ( 'NONE', #7495, .T. ) ;
#1578 = EDGE_LOOP ( 'NONE', ( #14590, #13725 ) ) ;
#1579 = DIRECTION ( 'NONE',  ( -0.000000000000000000, -0.000000000000000000, -1.000000000000000000 ) ) ;
#1580 = ORIENTED_EDGE ( 'NONE', *, *, #6702, .T. ) ;
#1581 = CARTESIAN_POINT ( 'NONE',  ( 10.40000000000000036, 0.000000000000000000, 0.000000000000000000 ) ) ;
#1582 = ORIENTED_EDGE ( 'NONE', *, *, #991, .T. ) ;
#1583 = CARTESIAN_POINT ( 'NONE',  ( 1.118033988749894458, 0.000000000000000000, 0.000000000000000000 ) ) ;
#1585 = CARTESIAN_POINT ( 'NONE',  ( -280.1255802622537203, 269.9854425596105898, 145.2906609804448124 ) ) ;
#1584 = B_SPLINE_CURVE_WITH_KNOTS ( 'NONE', 3,
 ( #12939, #20247, #6002, #2009, #22175, #13293, #18434, #337, #11243, #7702, #11467, #5646, #13054, #14961, #7572, #9399, #3697, #18556 ),
 .UNSPECIFIED., .F., .F.,
 ( 4, 2, 2, 2, 2, 2, 2, 2, 4 ),
 ( 0.5000000000000000000, 0.5625000000000000000, 0.6250000000000001110, 0.6875000000000001110, 0.7500000000000001110, 0.8125000000000001110, 0.8750000000000001110, 0.9375000000000000000, 1.000000000000000000 ),
 .UNSPECIFIED. ) ;
#1586 = EDGE_CURVE ( 'NONE', #12471, #4961, #8307, .T. ) ;
#1587 = DIRECTION ( 'NONE',  ( 0.000000000000000000, 0.000000000000000000, 1.000000000000000000 ) ) ;
#1588 = CARTESIAN_POINT ( 'NONE',  ( 124.6683470056595127, -1092.102735484117147, -32.49999999999354117 ) ) ;
#1589 = DIRECTION ( 'NONE',  ( 0.000000000000000000, 1.334402673828305746E-15, -1.000000000000000000 ) ) ;
#1590 = EDGE_LOOP ( 'NONE', ( #266, #2447 ) ) ;
#1591 = CARTESIAN_POINT ( 'NONE',  ( 145.0000000000000284, 0.000000000000000000, 90.00000000000000000 ) ) ;
#1593 = ORIENTED_EDGE ( 'NONE', *, *, #2778, .F. ) ;
#1592 = VERTEX_POINT ( 'NONE', #1660 ) ;
#1594 = DIRECTION ( 'NONE',  ( 0.000000000000000000, 0.000000000000000000, 1.000000000000000000 ) ) ;
#1595 = CARTESIAN_POINT ( 'NONE',  ( -137.9031948627971076, -44.80746418436799416, -90.00000000000000000 ) ) ;
#1596 = DIRECTION ( 'NONE',  ( -1.000000000000000000, -0.000000000000000000, -0.000000000000000000 ) ) ;
#1597 = ORIENTED_EDGE ( 'NONE', *, *, #13231, .F. ) ;
#1598 = CARTESIAN_POINT ( 'NONE',  ( -79.99999999999997158, -62.00000000000001421, 5.199999999999997513 ) ) ;
#1599 = LINE ( 'NONE', #12992, #15732 ) ;
#1600 = EDGE_LOOP ( 'NONE', ( #5028, #12753, #23276, #5091 ) ) ;
#1601 = ADVANCED_FACE ( 'NONE', ( #9043 ), #3478, .F. ) ;
#1602 = ADVANCED_FACE ( 'NONE', ( #1423 ), #18316, .F. ) ;
#1603 = CARTESIAN_POINT ( 'NONE',  ( 105.0000000000000000, -19.99999999999998934, 0.000000000000000000 ) ) ;
#1604 = CARTESIAN_POINT ( 'NONE',  ( 0.000000000000000000, 0.000000000000000000, 90.00000000000000000 ) ) ;
#1605 = CONTEXT_DEPENDENT_SHAPE_REPRESENTATION ( #15883, #20859 ) ;
#1606 = ORIENTED_EDGE ( 'NONE', *, *, #3413, .F. ) ;
#1607 = EDGE_LOOP ( 'NONE', ( #12718, #7709, #16085, #5672 ) ) ;
#1608 = CARTESIAN_POINT ( 'NONE',  ( 124.4701338314437891, -1092.369831568442805, 27.50000000000646239 ) ) ;
#1609 = ORIENTED_EDGE ( 'NONE', *, *, #2754, .F. ) ;
#1610 = CARTESIAN_POINT ( 'NONE',  ( -44.99999999999997868, -52.79999999999939320, 137.3500000000001648 ) ) ;
#1611 = EDGE_CURVE ( 'NONE', #21138, #9885, #12704, .T. ) ;
#1612 = CARTESIAN_POINT ( 'NONE',  ( 133.1760469597742542, 79.30426557766963924, 32.42079297023035167 ) ) ;
#1613 = CARTESIAN_POINT ( 'NONE',  ( 4.203935335434060505, 1.640780671294165272, -3.598452447879202598 ) ) ;
#1614 = ADVANCED_FACE ( 'NONE', ( #16516 ), #16777, .T. ) ;
#1615 = CARTESIAN_POINT ( 'NONE',  ( 235.0000000000000284, -557.0000000000000000, -60.00000000000000711 ) ) ;
#1616 = CARTESIAN_POINT ( 'NONE',  ( -79.99999999999997158, -62.00000000000001421, 5.199999999999997513 ) ) ;
#1617 = VERTEX_POINT ( 'NONE', #98 ) ;
#1618 = ADVANCED_FACE ( 'NONE', ( #7343, #14725 ), #23537, .T. ) ;
#1619 = CARTESIAN_POINT ( 'NONE',  ( 40.00000000000000000, 100.0000000000000000, 150.2000000000009550 ) ) ;
#1620 = DIRECTION ( 'NONE',  ( 1.000000000000000000, 0.000000000000000000, 0.000000000000000000 ) ) ;
#1621 = VERTEX_POINT ( 'NONE', #14596 ) ;
#1622 = DIRECTION ( 'NONE',  ( 0.000000000000000000, 1.000000000000000000, -0.000000000000000000 ) ) ;
#1623 = CARTESIAN_POINT ( 'NONE',  ( 70.00000000000000000, -112.6666666666666714, 0.000000000000000000 ) ) ;
#1624 = CIRCLE ( 'NONE', #13627, 2.649999999999985700 ) ;
#1625 = CARTESIAN_POINT ( 'NONE',  ( -285.2300000000000182, 267.7999999999999545, 146.4928932188134354 ) ) ;
#1626 = CARTESIAN_POINT ( 'NONE',  ( 3.000000000000002665, 0.000000000000000000, 0.000000000000000000 ) ) ;
#1627 = CARTESIAN_POINT ( 'NONE',  ( 280.8083875057488967, 271.2314821058791949, -148.9107452280323116 ) ) ;
#1628 = ORIENTED_EDGE ( 'NONE', *, *, #5078, .T. ) ;
#1629 = PLANE ( 'NONE',  #11213 ) ;
#1630 = ORIENTED_EDGE ( 'NONE', *, *, #4062, .T. ) ;
#1631 = CARTESIAN_POINT ( 'NONE',  ( -4.000000000000000000, 2.309401076758498483, -3.433295621305379353 ) ) ;
#1632 = DIRECTION ( 'NONE',  ( 1.000000000000000000, 0.000000000000000000, 0.000000000000000000 ) ) ;
#1633 = EDGE_CURVE ( 'NONE', #7326, #9978, #7511, .T. ) ;
#1634 = DIRECTION ( 'NONE',  ( 0.3090169943749589421, -0.9510565162951498674, 0.000000000000000000 ) ) ;
#1635 = EDGE_CURVE ( 'NONE', #4882, #20887, #19861, .T. ) ;
#1636 = ORIENTED_EDGE ( 'NONE', *, *, #15712, .T. ) ;
#1637 = SURFACE_STYLE_USAGE ( .BOTH. , #5620 ) ;
#1638 = CARTESIAN_POINT ( 'NONE',  ( 45.00000000000002132, -56.79999999999933635, 195.0000000000002274 ) ) ;
#1639 = EDGE_CURVE ( 'NONE', #1592, #2833, #13352, .T. ) ;
#1640 = LINE ( 'NONE', #21917, #39 ) ;
#1641 = CARTESIAN_POINT ( 'NONE',  ( 0.2500000000000002220, 0.000000000000000000, 0.000000000000000000 ) ) ;
#1642 = ADVANCED_FACE ( 'NONE', ( #1555, #7449 ), #14384, .T. ) ;
#1643 = LINE ( 'NONE', #3459, #13493 ) ;
#1644 = CARTESIAN_POINT ( 'NONE',  ( 80.00000000000004263, -137.9999999999999716, 3.000000000000000000 ) ) ;
#1645 = CARTESIAN_POINT ( 'NONE',  ( -20.63749999999999929, 0.000000000000000000, -21.02499999999999503 ) ) ;
#1646 = VECTOR ( 'NONE', #9901, 999.9999999999998863 ) ;
#1647 = VERTEX_POINT ( 'NONE', #6995 ) ;
#1648 = ADVANCED_FACE ( 'NONE', ( #21716 ), #5176, .T. ) ;
#1649 = EDGE_LOOP ( 'NONE', ( #11565, #23446, #13980, #11039 ) ) ;
#1650 = CARTESIAN_POINT ( 'NONE',  ( 0.000000000000000000, 1.865214261513747767E-15, 145.0000119999999697 ) ) ;
#1651 = FACE_OUTER_BOUND ( 'NONE', #10746, .T. ) ;
#1652 = EDGE_CURVE ( 'NONE', #16805, #2178, #14106, .T. ) ;
#1653 = ORIENTED_EDGE ( 'NONE', *, *, #17686, .F. ) ;
#1654 = DIRECTION ( 'NONE',  ( 0.000000000000000000, 2.618450529776326854E-15, 1.000000000000000000 ) ) ;
#1655 = DIRECTION ( 'NONE',  ( 0.000000000000000000, 0.000000000000000000, 1.000000000000000000 ) ) ;
#1656 = ORIENTED_EDGE ( 'NONE', *, *, #2894, .T. ) ;
#1657 = CARTESIAN_POINT ( 'NONE',  ( 280.1244266425809428, 269.9696999999999889, 145.2840560642353580 ) ) ;
#1658 = CARTESIAN_POINT ( 'NONE',  ( 80.00000000000004263, -137.9999999999999716, 3.000000000000000000 ) ) ;
#1659 = ORIENTED_EDGE ( 'NONE', *, *, #3677, .T. ) ;
#1660 = CARTESIAN_POINT ( 'NONE',  ( 45.00000000000002132, -56.79999999999935767, 137.3500000000002217 ) ) ;
#1661 = CARTESIAN_POINT ( 'NONE',  ( 52.00000000000000711, 0.000000000000000000, 0.000000000000000000 ) ) ;
#1662 = AXIS2_PLACEMENT_3D ( 'NONE', #5057, #9144, #22047 ) ;
#1663 = VERTEX_POINT ( 'NONE', #21944 ) ;
#1664 = EDGE_CURVE ( 'NONE', #21370, #4532, #16298, .T. ) ;
#1665 = FACE_OUTER_BOUND ( 'NONE', #16076, .T. ) ;
#1666 = CARTESIAN_POINT ( 'NONE',  ( -3.000000000000002665, 0.000000000000000000, 0.000000000000000000 ) ) ;
#1667 = DIRECTION ( 'NONE',  ( 1.000000000000000000, -3.051161311199799893E-31, -8.144298233840332611E-17 ) ) ;
#1668 = ORIENTED_EDGE ( 'NONE', *, *, #13168, .T. ) ;
#1669 = ORIENTED_EDGE ( 'NONE', *, *, #7701, .T. ) ;
#1670 = CARTESIAN_POINT ( 'NONE',  ( 284.5699028110927316, 270.4339272673396977, -145.9952621458755857 ) ) ;
#1671 = CARTESIAN_POINT ( 'NONE',  ( -126.4656051290183285, 89.61836744852109859, -29.67081494451417001 ) ) ;
#1672 = PLANE ( 'NONE',  #9200 ) ;
#1673 = CARTESIAN_POINT ( 'NONE',  ( 45.00000000000004974, -52.79999999999967741, 47.35000000000018616 ) ) ;
#1674 = VECTOR ( 'NONE', #9828, 1000.000000000000000 ) ;
#1675 = ORIENTED_EDGE ( 'NONE', *, *, #8013, .F. ) ;
#1676 = EDGE_CURVE ( 'NONE', #18305, #13461, #5588, .T. ) ;
#1677 = CARTESIAN_POINT ( 'NONE',  ( -37.68333333333335844, -89.99999999999997158, 3.000000000000000000 ) ) ;
#1678 = FILL_AREA_STYLE_COLOUR ( '', #3815 ) ;
#1679 = EDGE_CURVE ( 'NONE', #23662, #12107, #2064, .T. ) ;
#1680 = CARTESIAN_POINT ( 'NONE',  ( -90.00000000000000000, -94.99999999999998579, 3.000000000000000000 ) ) ;
#1681 = CARTESIAN_POINT ( 'NONE',  ( -79.99999999999995737, -59.79999999999998295, 5.199999999999989519 ) ) ;
#1682 = ORIENTED_EDGE ( 'NONE', *, *, #17229, .T. ) ;
#1683 =( REPRESENTATION_RELATIONSHIP ('NONE','NONE', #10127, #9771 ) REPRESENTATION_RELATIONSHIP_WITH_TRANSFORMATION ( #21413 )SHAPE_REPRESENTATION_RELATIONSHIP( ) );
#1684 = DIRECTION ( 'NONE',  ( -1.000000000000000000, -3.469446951953614682E-16, -0.000000000000000000 ) ) ;
#1685 = VECTOR ( 'NONE', #19508, 1000.000000000000000 ) ;
#1686 = VERTEX_POINT ( 'NONE', #6000 ) ;
#1687 = PRODUCT ( 'support structure', 'support structure', '', ( #5653 ) ) ;
#1688 = AXIS2_PLACEMENT_3D ( 'NONE', #10735, #16493, #17957 ) ;
#1689 = CARTESIAN_POINT ( 'NONE',  ( 2.700000000000001066, 0.000000000000000000, -25.00000000000000000 ) ) ;
#1690 = EDGE_LOOP ( 'NONE', ( #6686, #8215, #23216, #20846 ) ) ;
#1691 = LINE ( 'NONE', #1933, #20050 ) ;
#1692 = CARTESIAN_POINT ( 'NONE',  ( -124.2796999450275450, 81.25594874576316329, -29.99999999999356604 ) ) ;
#1693 = CARTESIAN_POINT ( 'NONE',  ( 7.500000000000001776, 0.000000000000000000, 0.000000000000000000 ) ) ;
#1694 = DIRECTION ( 'NONE',  ( 0.000000000000000000, -1.000000000000000000, 0.000000000000000000 ) ) ;
#1695 = EDGE_LOOP ( 'NONE', ( #19166, #21461, #15410, #19396 ) ) ;
#1696 = DIRECTION ( 'NONE',  ( -0.000000000000000000, -0.000000000000000000, -1.000000000000000000 ) ) ;
#1697 = SURFACE_STYLE_USAGE ( .BOTH. , #14528 ) ;
#1698 = AXIS2_PLACEMENT_3D ( 'NONE', #7708, #22425, #5886 ) ;
#1700 = ORIENTED_EDGE ( 'NONE', *, *, #10708, .F. ) ;
#1699 = VERTEX_POINT ( 'NONE', #9396 ) ;
#1701 = VECTOR ( 'NONE', #22770, 1000.000000000000000 ) ;
#1702 = CARTESIAN_POINT ( 'NONE',  ( 45.00000000000000000, 283.0000000000000000, 0.000000000000000000 ) ) ;
#1703 = LINE ( 'NONE', #16446, #1543 ) ;
#1704 = DIRECTION ( 'NONE',  ( 0.000000000000000000, 0.000000000000000000, -1.000000000000000000 ) ) ;
#1705 = ORIENTED_EDGE ( 'NONE', *, *, #18577, .F. ) ;
#1706 = FACE_OUTER_BOUND ( 'NONE', #17410, .T. ) ;
#1707 = CARTESIAN_POINT ( 'NONE',  ( -44.99999999999997868, -52.79999999999938609, 140.0000000000001421 ) ) ;
#1708 = EDGE_LOOP ( 'NONE', ( #1630, #19330 ) ) ;
#1709 = LINE ( 'NONE', #14329, #18113 ) ;
#1710 = DIRECTION ( 'NONE',  ( 1.000000000000000000, 0.000000000000000000, 0.000000000000000000 ) ) ;
#1711 = CONTEXT_DEPENDENT_SHAPE_REPRESENTATION ( #13623, #9877 ) ;
#1712 = ORIENTED_EDGE ( 'NONE', *, *, #6318, .T. ) ;
#1713 = EDGE_LOOP ( 'NONE', ( #20461, #7584, #11556, #5521, #1659 ) ) ;
#1714 = CARTESIAN_POINT ( 'NONE',  ( -282.2000000000013529, -89.99999999999896261, -40.33333333333332860 ) ) ;
#1715 = VERTEX_POINT ( 'NONE', #9760 ) ;
#1716 = CARTESIAN_POINT ( 'NONE',  ( -129.1746529357998270, 85.66745698985749868, 28.88700448195642068 ) ) ;
#1717 = CARTESIAN_POINT ( 'NONE',  ( 5.000000000000000000, 0.000000000000000000, 0.000000000000000000 ) ) ;
#1718 = AXIS2_PLACEMENT_3D ( 'NONE', #14058, #10435, #15617 ) ;
#1719 = DIRECTION ( 'NONE',  ( -0.000000000000000000, -0.000000000000000000, 1.000000000000000000 ) ) ;
#1720 = AXIS2_PLACEMENT_3D ( 'NONE', #3933, #5997, #18550 ) ;
#1721 = DIRECTION ( 'NONE',  ( 0.000000000000000000, 0.000000000000000000, 1.000000000000000000 ) ) ;
#1722 = DIRECTION ( 'NONE',  ( 0.6568457881071740889, 0.2618274444092085762, -0.7071067811865532349 ) ) ;
#1723 = ORIENTED_EDGE ( 'NONE', *, *, #14907, .T. ) ;
#1724 = EDGE_CURVE ( 'NONE', #16388, #15256, #334, .T. ) ;
#1725 = DIRECTION ( 'NONE',  ( 0.000000000000000000, 0.000000000000000000, 1.000000000000000000 ) ) ;
#1726 = CARTESIAN_POINT ( 'NONE',  ( 0.000000000000000000, 0.000000000000000000, -0.2800830152838844622 ) ) ;
#1727 = CARTESIAN_POINT ( 'NONE',  ( 7.908030677224553884, -3.059924800338349904, -7.792662696733364314 ) ) ;
#1728 = ADVANCED_FACE ( 'NONE', ( #13407 ), #1345, .T. ) ;
#1729 = EDGE_CURVE ( 'NONE', #14202, #15482, #20862, .T. ) ;
#1730 = ORIENTED_EDGE ( 'NONE', *, *, #1871, .F. ) ;
#1731 = LINE ( 'NONE', #7301, #9257 ) ;
#1732 = FACE_BOUND ( 'NONE', #9168, .T. ) ;
#1733 = EDGE_CURVE ( 'NONE', #12392, #6476, #21523, .T. ) ;
#1734 = CARTESIAN_POINT ( 'NONE',  ( -284.1822575857425477, 271.0140793454687582, 145.8708543776411659 ) ) ;
#1735 = CLOSED_SHELL ( 'NONE', ( #13363, #16071, #9628, #22127, #8705, #21441, #8757, #1602, #22748, #9080, #14947, #13025, #14476, #19578, #2546, #7223, #10942, #8896, #15552, #7130, #7059, #20518, #17509, #23348, #23768, #9961, #14916, #18560, #153, #2149, #3503, #816, #18070, #11756, #10182, #7282, #6829, #11757, #23281, #7968, #2240, #22742, #18986, #7336, #15830, #911, #9920, #22834, #16286, #22037, #12930, #23177, #7926, #19756, #3416, #16865, #6167, #17306, #11112, #15935, #9576, #16560, #742, #10355, #5623, #4008, #17245, #9140, #5438, #18901, #2071, #16252, #20434, #12891, #9756, #17939, #8043, #12470, #15163, #17696, #12959, #9190, #8118, #16640, #23620, #18287, #16603, #2687, #21080, #8934, #2478, #18885, #21715, #6232, #3886, #7532, #2388, #10074, #11374, #13764, #18244, #4455, #21245, #5079 ) ) ;
#1736 = DIRECTION ( 'NONE',  ( -0.000000000000000000, -0.000000000000000000, 1.000000000000000000 ) ) ;
#1737 = DIRECTION ( 'NONE',  ( 0.000000000000000000, -0.000000000000000000, 1.000000000000000000 ) ) ;
#1738 = ORIENTED_EDGE ( 'NONE', *, *, #15643, .F. ) ;
#1739 = DIRECTION ( 'NONE',  ( 1.000000000000000000, -0.000000000000000000, -0.000000000000000000 ) ) ;
#1740 = EDGE_LOOP ( 'NONE', ( #20447, #18390, #7293, #13753 ) ) ;
#1741 = CARTESIAN_POINT ( 'NONE',  ( 145.0000000000000284, 1.518794382396763073E-12, -90.00000000000000000 ) ) ;
#1742 = CIRCLE ( 'NONE', #21820, 4.250000000000000000 ) ;
#1743 = LINE ( 'NONE', #15064, #4801 ) ;
#1744 = ORIENTED_EDGE ( 'NONE', *, *, #6460, .T. ) ;
#1745 = CARTESIAN_POINT ( 'NONE',  ( 124.0809974055272704, -1092.892044598690291, -32.42132972170173133 ) ) ;
#1746 = VECTOR ( 'NONE', #9787, 1000.000000000000000 ) ;
#1747 = DIRECTION ( 'NONE',  ( 0.000000000000000000, 0.000000000000000000, 1.000000000000000000 ) ) ;
#1748 = DIRECTION ( 'NONE',  ( 1.000000000000000000, 0.000000000000000000, 0.000000000000000000 ) ) ;
#1749 = CARTESIAN_POINT ( 'NONE',  ( 5.000000000000001776, 6.123233995736768255E-16, -9.974600000000000577 ) ) ;
#1750 = DIRECTION ( 'NONE',  ( 1.000000000000000000, 0.000000000000000000, 0.000000000000000000 ) ) ;
#1751 = FACE_OUTER_BOUND ( 'NONE', #21991, .T. ) ;
#1752 = CIRCLE ( 'NONE', #22195, 2.649999999999999467 ) ;
#1753 = EDGE_LOOP ( 'NONE', ( #14529, #14866, #3158, #19813, #833 ) ) ;
#1754 = VERTEX_POINT ( 'NONE', #14958 ) ;
#1755 = DIRECTION ( 'NONE',  ( 0.000000000000000000, -3.495664435217746987E-15, -1.000000000000000000 ) ) ;
#1756 = DIRECTION ( 'NONE',  ( 0.000000000000000000, 0.000000000000000000, -1.000000000000000000 ) ) ;
#1757 = EDGE_LOOP ( 'NONE', ( #8882, #20556, #17821, #15590, #12226, #23679, #18207, #10724, #1419, #19201, #18727 ) ) ;
#1758 = EDGE_CURVE ( 'NONE', #10543, #11584, #3381, .T. ) ;
#1759 = CARTESIAN_POINT ( 'NONE',  ( -1.500000000000000000, 12.00000000000000000, -50.00000000000000000 ) ) ;
#1760 = DIRECTION ( 'NONE',  ( -1.000000000000000000, 0.000000000000000000, 0.000000000000000000 ) ) ;
#1761 = AXIS2_PLACEMENT_3D ( 'NONE', #19347, #17542, #21521 ) ;
#1762 = EDGE_CURVE ( 'NONE', #13072, #14205, #10366, .T. ) ;
#1763 = VERTEX_POINT ( 'NONE', #3936 ) ;
#1764 = CYLINDRICAL_SURFACE ( 'NONE', #5955, 2.649999999999999467 ) ;
#1765 = EDGE_CURVE ( 'NONE', #16905, #21880, #22652, .T. ) ;
#1766 = CARTESIAN_POINT ( 'NONE',  ( 1.567478505476134606E-15, 4.618802153517012066, -3.433295621305382905 ) ) ;
#1767 = ORIENTED_EDGE ( 'NONE', *, *, #15455, .F. ) ;
#1768 = DIRECTION ( 'NONE',  ( 0.000000000000000000, -1.000000000000000000, -3.172065784643303781E-15 ) ) ;
#1769 = DIRECTION ( 'NONE',  ( 0.000000000000000000, 0.000000000000000000, 1.000000000000000000 ) ) ;
#1770 = ADVANCED_FACE ( 'NONE', ( #7937 ), #18780, .T. ) ;
#1771 = LINE ( 'NONE', #15201, #16938 ) ;
#1772 = ORIENTED_EDGE ( 'NONE', *, *, #17021, .F. ) ;
#1773 = DIRECTION ( 'NONE',  ( 0.000000000000000000, -0.5000000000000009992, -0.8660254037844380415 ) ) ;
#1775 = EDGE_CURVE ( 'NONE', #7126, #6529, #9987, .T. ) ;
#1774 = CARTESIAN_POINT ( 'NONE',  ( -135.8696211158498386, -1074.595399753385209, 27.50000000000646949 ) ) ;
#1776 = CARTESIAN_POINT ( 'NONE',  ( 2.500000000000000000, 2.357898499370433054, -1.951563910473907981E-15 ) ) ;
#1777 = EDGE_LOOP ( 'NONE', ( #3273, #11325, #13086, #16443 ) ) ;
#1778 = ORIENTED_EDGE ( 'NONE', *, *, #7984, .T. ) ;
#1779 = CARTESIAN_POINT ( 'NONE',  ( 1.500000000000001332, 0.000000000000000000, 0.000000000000000000 ) ) ;
#1780 = PRODUCT_DEFINITION_SHAPE ( 'NONE', 'NONE',  #23891 ) ;
#1781 = SHAPE_DEFINITION_REPRESENTATION ( #5553, #18083 ) ;
#1782 = PLANE ( 'NONE',  #6580 ) ;
#1783 = AXIS2_PLACEMENT_3D ( 'NONE', #13110, #11294, #20425 ) ;
#1784 = CARTESIAN_POINT ( 'NONE',  ( 0.000000000000000000, 0.000000000000000000, -90.00000000000000000 ) ) ;
#1785 = VERTEX_POINT ( 'NONE', #14685 ) ;
#1786 = LINE ( 'NONE', #12951, #18991 ) ;
#1787 = ORIENTED_EDGE ( 'NONE', *, *, #4137, .F. ) ;
#1788 = CARTESIAN_POINT ( 'NONE',  ( -12.52876685377503385, -21.69578997558839717, 145.0000119999999981 ) ) ;
#1789 = PRODUCT_DEFINITION_CONTEXT ( 'detailed design', #19235, 'design' ) ;
#1790 = CIRCLE ( 'NONE', #9160, 2.500000000000002220 ) ;
#1791 = DIRECTION ( 'NONE',  ( 0.000000000000000000, -0.000000000000000000, 1.000000000000000000 ) ) ;
#1792 = CARTESIAN_POINT ( 'NONE',  ( -44.99999999999995026, -52.79999999999969873, 50.00000000000018474 ) ) ;
#1793 = ORIENTED_EDGE ( 'NONE', *, *, #20489, .F. ) ;
#1794 = AXIS2_PLACEMENT_3D ( 'NONE', #14987, #11136, #18938 ) ;
#1795 = CARTESIAN_POINT ( 'NONE',  ( -6.127431526422343306E-17, 9.147862274876549904, -8.047472243342932430 ) ) ;
#1796 = VERTEX_POINT ( 'NONE', #2374 ) ;
#1797 = ADVANCED_FACE ( 'NONE', ( #15318 ), #17117, .T. ) ;
#1798 = ADVANCED_FACE ( 'NONE', ( #16753 ), #11465, .F. ) ;
#1799 = DIRECTION ( 'NONE',  ( 0.000000000000000000, 1.000000000000000000, -3.502807018799300809E-15 ) ) ;
#1800 = ADVANCED_FACE ( 'NONE', ( #214, #573 ), #4314, .F. ) ;
#1801 = CARTESIAN_POINT ( 'NONE',  ( 80.00000000000000000, -61.99999999999998579, 0.000000000000000000 ) ) ;
#1802 = ORIENTED_EDGE ( 'NONE', *, *, #11955, .F. ) ;
#1803 = FACE_OUTER_BOUND ( 'NONE', #9769, .T. ) ;
#1804 = PLANE ( 'NONE',  #15058 ) ;
#1805 = CIRCLE ( 'NONE', #6059, 21.50000000000000000 ) ;
#1806 = PLANE ( 'NONE',  #4570 ) ;
#1807 =( REPRESENTATION_RELATIONSHIP ('NONE','NONE', #10127, #3124 ) REPRESENTATION_RELATIONSHIP_WITH_TRANSFORMATION ( #8513 )SHAPE_REPRESENTATION_RELATIONSHIP( ) );
#1808 = CYLINDRICAL_SURFACE ( 'NONE', #23222, 2.649999999999999467 ) ;
#1809 = DIRECTION ( 'NONE',  ( 0.000000000000000000, 0.000000000000000000, 1.000000000000000000 ) ) ;
#1810 = ORIENTED_EDGE ( 'NONE', *, *, #19149, .F. ) ;
#1811 = LINE ( 'NONE', #9206, #10408 ) ;
#1812 = VECTOR ( 'NONE', #22970, 1000.000000000000000 ) ;
#1813 = DIRECTION ( 'NONE',  ( 1.751623080406021339E-46, 3.469446951953613794E-15, 1.000000000000000000 ) ) ;
#1814 =( LENGTH_UNIT ( ) NAMED_UNIT ( * ) SI_UNIT ( .MILLI., .METRE. ) );
#1815 = AXIS2_PLACEMENT_3D ( 'NONE', #8788, #21805, #10733 ) ;
#1817 = EDGE_LOOP ( 'NONE', ( #14714, #23618 ) ) ;
#1816 = VERTEX_POINT ( 'NONE', #16868 ) ;
#1818 = DIRECTION ( 'NONE',  ( 1.000000000000000000, 0.000000000000000000, 0.000000000000000000 ) ) ;
#1819 = DIRECTION ( 'NONE',  ( 0.000000000000000000, 1.000000000000000000, -1.287488025362403787E-15 ) ) ;
#1820 = CARTESIAN_POINT ( 'NONE',  ( 280.1244266425809428, 269.9697000000000457, -145.2840560642351875 ) ) ;
#1821 = VERTEX_POINT ( 'NONE', #7699 ) ;
#1822 = DIRECTION ( 'NONE',  ( -1.000000000000000000, -0.000000000000000000, -0.000000000000000000 ) ) ;
#1823 = FACE_OUTER_BOUND ( 'NONE', #12229, .T. ) ;
#1824 = ORIENTED_EDGE ( 'NONE', *, *, #17434, .T. ) ;
#1825 = EDGE_CURVE ( 'NONE', #13236, #17386, #21895, .T. ) ;
#1826 = AXIS2_PLACEMENT_3D ( 'NONE', #9456, #16809, #18720 ) ;
#1827 = CARTESIAN_POINT ( 'NONE',  ( -135.4018704341557680, 51.87806360044768184, -2.775557561562891351E-14 ) ) ;
#1828 = LINE ( 'NONE', #5350, #21940 ) ;
#1829 = CIRCLE ( 'NONE', #15362, 4.250000000000000000 ) ;
#1830 = ORIENTED_EDGE ( 'NONE', *, *, #19679, .T. ) ;
#1831 = EDGE_CURVE ( 'NONE', #9606, #13337, #14784, .T. ) ;
#1832 = CARTESIAN_POINT ( 'NONE',  ( 0.000000000000000000, 0.000000000000000000, -5.000000000000000000 ) ) ;
#1833 = ORIENTED_EDGE ( 'NONE', *, *, #9070, .T. ) ;
#1834 = CARTESIAN_POINT ( 'NONE',  ( 2.500000000000000000, -1.768423874527825568, -1.020999999999998575 ) ) ;
#1835 = CARTESIAN_POINT ( 'NONE',  ( 133.2566323304055800, 79.16876461166395984, 27.62610291900640291 ) ) ;
#1836 = CARTESIAN_POINT ( 'NONE',  ( 4.197478902586992966, -0.8524102783748346290, -3.505063281295504041 ) ) ;
#1837 = DIRECTION ( 'NONE',  ( 0.000000000000000000, 1.000000000000000000, -1.287488025362403787E-15 ) ) ;
#1838 = CARTESIAN_POINT ( 'NONE',  ( 89.00000000000000000, -149.9999999999996874, 129.9038105676659711 ) ) ;
#1839 = CARTESIAN_POINT ( 'NONE',  ( -1.500000000000000000, 9.886859966642592923, -50.00000000000000000 ) ) ;
#1840 = EDGE_LOOP ( 'NONE', ( #23285, #20964 ) ) ;
#1841 = CARTESIAN_POINT ( 'NONE',  ( -362.5513232148721841, -379.7124412435653085, 0.000000000000000000 ) ) ;
#1842 = CIRCLE ( 'NONE', #15376, 5.000000000000001776 ) ;
#1843 = DIRECTION ( 'NONE',  ( 5.135813185032629306E-32, -1.850371707708594366E-15, -1.000000000000000000 ) ) ;
#1844 = CARTESIAN_POINT ( 'NONE',  ( -5.007715329123872641E-16, -8.660254037844399733, -7.422398894150038728 ) ) ;
#1845 = VECTOR ( 'NONE', #954, 1000.000000000000000 ) ;
#1846 = ORIENTED_EDGE ( 'NONE', *, *, #10977, .T. ) ;
#1847 = CIRCLE ( 'NONE', #22280, 2.200000000000028155 ) ;
#1848 = CARTESIAN_POINT ( 'NONE',  ( -282.2000000000008981, 35.00000000000100897, 105.0000000000000000 ) ) ;
#1849 = CARTESIAN_POINT ( 'NONE',  ( 45.00000000000000711, 5.510910596163090344E-15, 169.9999999999999716 ) ) ;
#1850 = EDGE_CURVE ( 'NONE', #11584, #22213, #9574, .T. ) ;
#1851 = DIRECTION ( 'NONE',  ( -1.000000000000000000, 0.000000000000000000, 0.000000000000000000 ) ) ;
#1852 = DIRECTION ( 'NONE',  ( -0.000000000000000000, -0.000000000000000000, 1.000000000000000000 ) ) ;
#1853 = DIRECTION ( 'NONE',  ( 1.000000000000000000, 0.000000000000000000, 0.000000000000000000 ) ) ;
#1854 = ORIENTED_EDGE ( 'NONE', *, *, #9075, .T. ) ;
#1855 = DIRECTION ( 'NONE',  ( 0.000000000000000000, 2.618450529776313049E-15, 1.000000000000000000 ) ) ;
#1856 = ORIENTED_EDGE ( 'NONE', *, *, #20103, .F. ) ;
#1857 = EDGE_CURVE ( 'NONE', #8155, #19239, #16024, .T. ) ;
#1859 = CARTESIAN_POINT ( 'NONE',  ( 5.200000000000002842, 0.000000000000000000, 0.000000000000000000 ) ) ;
#1858 = CONICAL_SURFACE ( 'NONE', #8061, 7.500000000000001776, 0.8594454914424796144 ) ;
#1860 = VECTOR ( 'NONE', #5273, 1000.000000000000114 ) ;
#1861 = DIRECTION ( 'NONE',  ( 0.000000000000000000, 0.000000000000000000, -1.000000000000000000 ) ) ;
#1862 = EDGE_CURVE ( 'NONE', #23140, #13840, #11917, .T. ) ;
#1863 = AXIS2_PLACEMENT_3D ( 'NONE', #5506, #11334, #20339 ) ;
#1864 = VERTEX_POINT ( 'NONE', #12196 ) ;
#1865 = LINE ( 'NONE', #21914, #7643 ) ;
#1866 = AXIS2_PLACEMENT_3D ( 'NONE', #21039, #4499, #11907 ) ;
#1867 = CARTESIAN_POINT ( 'NONE',  ( 123.0250976530550133, -1094.285891978964401, -29.19154146838977226 ) ) ;
#1868 = CARTESIAN_POINT ( 'NONE',  ( -155.0000000000000284, -1000.000000000000000, -90.00000000000000000 ) ) ;
#1869 = CARTESIAN_POINT ( 'NONE',  ( -281.4928932188134354, -129.2000000000000455, -177.2000000000013529 ) ) ;
#1870 = PLANE ( 'NONE',  #10772 ) ;
#1871 = EDGE_CURVE ( 'NONE', #12413, #8456, #8408, .T. ) ;
#1872 = FACE_OUTER_BOUND ( 'NONE', #23417, .T. ) ;
#1873 = LINE ( 'NONE', #22157, #4371 ) ;
#1874 = ORIENTED_EDGE ( 'NONE', *, *, #16107, .F. ) ;
#1875 = ORIENTED_EDGE ( 'NONE', *, *, #2102, .F. ) ;
#1876 = DIRECTION ( 'NONE',  ( 0.8090169943749468962, 0.5877852522924740253, 0.000000000000000000 ) ) ;
#1877 = DIRECTION ( 'NONE',  ( -1.000000000000000000, 0.000000000000000000, 0.000000000000000000 ) ) ;
#1878 = ORIENTED_EDGE ( 'NONE', *, *, #3277, .T. ) ;
#1879 = PRODUCT_DEFINITION_SHAPE ( 'NONE', 'NONE',  #4601 ) ;
#1880 = CARTESIAN_POINT ( 'NONE',  ( 6.811259022622480508, 7.416704320018591368, 200.0000120000000550 ) ) ;
#1881 = CARTESIAN_POINT ( 'NONE',  ( 7.298354728637812983, -4.926141412639873707, -7.913704048099693189 ) ) ;
#1882 = AXIS2_PLACEMENT_3D ( 'NONE', #10560, #10088, #17428 ) ;
#1883 = AXIS2_PLACEMENT_3D ( 'NONE', #17096, #15181, #18896 ) ;
#1884 = VECTOR ( 'NONE', #3181, 1000.000000000000000 ) ;
#1885 = AXIS2_PLACEMENT_3D ( 'NONE', #1848, #5137, #12796 ) ;
#1886 = CARTESIAN_POINT ( 'NONE',  ( 279.9999999999999432, 269.9999999999999432, 145.0000000000000284 ) ) ;
#1887 = VECTOR ( 'NONE', #1959, 1000.000000000000000 ) ;
#1888 = VECTOR ( 'NONE', #20864, 1000.000000000000000 ) ;
#1889 = EDGE_LOOP ( 'NONE', ( #14035, #13919, #9509, #20790 ) ) ;
#1890 = DIRECTION ( 'NONE',  ( -1.000000000000000000, 0.000000000000000000, -0.000000000000000000 ) ) ;
#1891 = CARTESIAN_POINT ( 'NONE',  ( 4.606548227981508425, 6.456511556909250160, -7.591235721156633254 ) ) ;
#1892 = CARTESIAN_POINT ( 'NONE',  ( -121.5574576620394112, -79.04925354955290118, 90.00000000000000000 ) ) ;
#1893 = VERTEX_POINT ( 'NONE', #6831 ) ;
#1894 = EDGE_CURVE ( 'NONE', #4011, #20488, #1166, .T. ) ;
#1895 = CARTESIAN_POINT ( 'NONE',  ( 45.00000000000004974, -52.79999999999966320, 52.65000000000017621 ) ) ;
#1896 = DIRECTION ( 'NONE',  ( 0.000000000000000000, -1.000000000000000000, 0.000000000000000000 ) ) ;
#1897 = EDGE_CURVE ( 'NONE', #17629, #8807, #23245, .T. ) ;
#1898 = ORIENTED_EDGE ( 'NONE', *, *, #3129, .T. ) ;
#1899 = ORIENTED_EDGE ( 'NONE', *, *, #8577, .F. ) ;
#1900 = DIRECTION ( 'NONE',  ( -1.000000000000000000, -0.000000000000000000, -0.000000000000000000 ) ) ;
#1901 = APPLICATION_PROTOCOL_DEFINITION ( 'draft international standard', 'automotive_design', 1998, #20934 ) ;
#1902 = DIRECTION ( 'NONE',  ( 0.000000000000000000, 0.5000000000000011102, 0.8660254037844379305 ) ) ;
#1904 = VECTOR ( 'NONE', #5428, 1000.000000000000000 ) ;
#1903 = AXIS2_PLACEMENT_3D ( 'NONE', #15044, #424, #22245 ) ;
#1905 = ADVANCED_FACE ( 'NONE', ( #1273 ), #8190, .F. ) ;
#1907 = DIRECTION ( 'NONE',  ( -0.000000000000000000, -0.000000000000000000, 1.000000000000000000 ) ) ;
#1906 =( GEOMETRIC_REPRESENTATION_CONTEXT ( 3 ) GLOBAL_UNCERTAINTY_ASSIGNED_CONTEXT ( ( #469 ) ) GLOBAL_UNIT_ASSIGNED_CONTEXT ( ( #4859, #14311, #1108 ) ) REPRESENTATION_CONTEXT ( 'NONE', 'WORKASPACE' ) );
#1908 = CARTESIAN_POINT ( 'NONE',  ( -137.9031948627974486, 44.80746418436699940, -90.00000000000000000 ) ) ;
#1909 = B_SPLINE_CURVE_WITH_KNOTS ( 'NONE', 3,
 ( #216, #13185, #11110, #22420, #20486, #1891, #13291, #9517, #3581, #10997 ),
 .UNSPECIFIED., .F., .F.,
 ( 4, 2, 2, 2, 4 ),
 ( 1.572453990175171705E-19, 0.002305503304226491201, 0.004611006608452982401, 0.006916509912679473168, 0.009222013216905964803 ),
 .UNSPECIFIED. ) ;
#1910 = CIRCLE ( 'NONE', #9647, 7.499999999999998224 ) ;
#1911 = EDGE_CURVE ( 'NONE', #17693, #2497, #16893, .T. ) ;
#1912 = ORIENTED_EDGE ( 'NONE', *, *, #7800, .F. ) ;
#1913 = LINE ( 'NONE', #14861, #19155 ) ;
#1914 = ADVANCED_FACE ( 'NONE', ( #17471, #916 ), #21219, .T. ) ;
#1915 = PRODUCT_RELATED_PRODUCT_CATEGORY ( 'part', '', ( #3604 ) ) ;
#1916 = ADVANCED_FACE ( 'NONE', ( #15095 ), #12665, .F. ) ;
#1917 = UNCERTAINTY_MEASURE_WITH_UNIT (LENGTH_MEASURE( 1.000000000000000082E-05 ), #22409, 'distance_accuracy_value', 'NONE');
#1918 = EDGE_LOOP ( 'NONE', ( #7609, #8535, #973, #13571 ) ) ;
#1919 = DIRECTION ( 'NONE',  ( 1.000000000000000000, 2.775557561562891351E-17, 0.000000000000000000 ) ) ;
#1920 = DIRECTION ( 'NONE',  ( 0.000000000000000000, 0.000000000000000000, 1.000000000000000000 ) ) ;
#1921 = LINE ( 'NONE', #8945, #22502 ) ;
#1922 = ORIENTED_EDGE ( 'NONE', *, *, #14781, .F. ) ;
#1923 = DIRECTION ( 'NONE',  ( 0.000000000000000000, 1.224646799147357891E-16, 1.000000000000000000 ) ) ;
#1924 =( GEOMETRIC_REPRESENTATION_CONTEXT ( 3 ) GLOBAL_UNCERTAINTY_ASSIGNED_CONTEXT ( ( #2665 ) ) GLOBAL_UNIT_ASSIGNED_CONTEXT ( ( #1814, #2662, #15492 ) ) REPRESENTATION_CONTEXT ( 'NONE', 'WORKASPACE' ) );
#1925 = AXIS2_PLACEMENT_3D ( 'NONE', #11459, #17111, #17003 ) ;
#1926 = CIRCLE ( 'NONE', #15467, 2.199999999999979750 ) ;
#1927 = CIRCLE ( 'NONE', #13566, 23.50000000000000000 ) ;
#1928 = VERTEX_POINT ( 'NONE', #16265 ) ;
#1929 = DIRECTION ( 'NONE',  ( 0.000000000000000000, 0.4999999999999979461, -0.8660254037844397068 ) ) ;
#1930 = CARTESIAN_POINT ( 'NONE',  ( 17.00000000000000000, 2.789133085058097101E-16, -2.055000000000000160 ) ) ;
#1931 = ORIENTED_EDGE ( 'NONE', *, *, #14365, .T. ) ;
#1932 = DIRECTION ( 'NONE',  ( 1.000000000000000000, 0.000000000000000000, -0.000000000000000000 ) ) ;
#1933 = CARTESIAN_POINT ( 'NONE',  ( -24.99999999999995381, -52.79999999999975557, 35.00000000000017764 ) ) ;
#1934 = EDGE_CURVE ( 'NONE', #17283, #16779, #5492, .T. ) ;
#1935 =( NAMED_UNIT ( * ) PLANE_ANGLE_UNIT ( ) SI_UNIT ( $, .RADIAN. ) );
#1936 = CARTESIAN_POINT ( 'NONE',  ( -282.2000000000000455, 267.7999999999999545, -146.4928932188134354 ) ) ;
#1937 = CARTESIAN_POINT ( 'NONE',  ( 125.4586218058184670, -1091.022788359629203, -31.88744336596587559 ) ) ;
#1938 = CARTESIAN_POINT ( 'NONE',  ( 99.99999999999987210, -127.0000000000000853, 147.2000000000013529 ) ) ;
#1939 = ORIENTED_EDGE ( 'NONE', *, *, #5439, .F. ) ;
#1940 = EDGE_CURVE ( 'NONE', #10258, #9956, #8997, .T. ) ;
#1941 = EDGE_CURVE ( 'NONE', #17109, #11264, #3550, .T. ) ;
#1942 = PLANE ( 'NONE',  #4124 ) ;
#1943 = LINE ( 'NONE', #5686, #11472 ) ;
#1945 = ORIENTED_EDGE ( 'NONE', *, *, #21631, .F. ) ;
#1944 = ORIENTED_EDGE ( 'NONE', *, *, #8240, .T. ) ;
#1946 = EDGE_CURVE ( 'NONE', #493, #784, #2228, .T. ) ;
#1947 = DIRECTION ( 'NONE',  ( 0.9237280213470682178, 0.3830490080632377725, 1.131240564625405124E-16 ) ) ;
#1948 = ADVANCED_FACE ( 'NONE', ( #5038 ), #3192, .F. ) ;
#1949 = CARTESIAN_POINT ( 'NONE',  ( -135.8686487629348676, -1074.597166325825583, -27.49999999999351985 ) ) ;
#1950 = DIRECTION ( 'NONE',  ( -0.000000000000000000, -0.000000000000000000, 1.000000000000000000 ) ) ;
#1951 = EDGE_CURVE ( 'NONE', #20344, #18305, #14697, .T. ) ;
#1952 = ORIENTED_EDGE ( 'NONE', *, *, #22528, .T. ) ;
#1953 = CARTESIAN_POINT ( 'NONE',  ( -134.6139742523213272, -1076.838024977515715, 30.81384172145502731 ) ) ;
#1954 = EDGE_LOOP ( 'NONE', ( #7032, #3935, #21847, #5928, #4847 ) ) ;
#1955 = CARTESIAN_POINT ( 'NONE',  ( -90.00000000000000000, -74.99999999999998579, 0.000000000000000000 ) ) ;
#1956 = VERTEX_POINT ( 'NONE', #10856 ) ;
#1957 = DIRECTION ( 'NONE',  ( -0.000000000000000000, -0.000000000000000000, 1.000000000000000000 ) ) ;
#1958 =( REPRESENTATION_RELATIONSHIP ('NONE','NONE', #10127, #11474 ) REPRESENTATION_RELATIONSHIP_WITH_TRANSFORMATION ( #8000 )SHAPE_REPRESENTATION_RELATIONSHIP( ) );
#1959 = DIRECTION ( 'NONE',  ( -0.000000000000000000, -0.000000000000000000, 1.000000000000000000 ) ) ;
#1960 = CONTEXT_DEPENDENT_SHAPE_REPRESENTATION ( #16059, #5456 ) ;
#1961 = ORIENTED_EDGE ( 'NONE', *, *, #21494, .T. ) ;
#1962 = LINE ( 'NONE', #5240, #17573 ) ;
#1963 = VERTEX_POINT ( 'NONE', #12446 ) ;
#1964 = CARTESIAN_POINT ( 'NONE',  ( -129.0286178947084466, 85.88727694560715520, 28.47118012353584859 ) ) ;
#1965 = CARTESIAN_POINT ( 'NONE',  ( 80.00000000000001421, -56.79999999999998295, 5.199999999999985967 ) ) ;
#1966 = CARTESIAN_POINT ( 'NONE',  ( -6.473970235329672780E-16, -4.862606272033106691, -3.745885042887442395 ) ) ;
#1967 = DIRECTION ( 'NONE',  ( 0.000000000000000000, 1.000000000000000000, 0.000000000000000000 ) ) ;
#1968 = CARTESIAN_POINT ( 'NONE',  ( 45.00000000000002132, -52.79999999999935767, 142.6500000000002046 ) ) ;
#1969 = DIRECTION ( 'NONE',  ( 0.000000000000000000, 0.8660254037844380415, -0.5000000000000012212 ) ) ;
#1970 = ORIENTED_EDGE ( 'NONE', *, *, #15943, .T. ) ;
#1971 = CARTESIAN_POINT ( 'NONE',  ( 0.000000000000000000, 0.000000000000000000, 0.000000000000000000 ) ) ;
#1972 = EDGE_CURVE ( 'NONE', #19310, #20612, #19745, .T. ) ;
#1973 = DIRECTION ( 'NONE',  ( 0.000000000000000000, -3.491481338843133355E-15, -1.000000000000000000 ) ) ;
#1974 = LINE ( 'NONE', #2088, #1183 ) ;
#1975 = EDGE_CURVE ( 'NONE', #3512, #8656, #1082, .T. ) ;
#1976 = ORIENTED_EDGE ( 'NONE', *, *, #4096, .F. ) ;
#1977 = ADVANCED_FACE ( 'NONE', ( #5259 ), #11076, .F. ) ;
#1978 = CARTESIAN_POINT ( 'NONE',  ( 155.0000000000000284, -500.0000000000000000, -32.49999999999997158 ) ) ;
#1979 = LINE ( 'NONE', #16836, #16431 ) ;
#1980 = CARTESIAN_POINT ( 'NONE',  ( 155.0000000000000284, -500.0000000000000000, 27.50000000000001066 ) ) ;
#1981 = DIRECTION ( 'NONE',  ( 0.000000000000000000, -0.000000000000000000, 1.000000000000000000 ) ) ;
#1982 = CARTESIAN_POINT ( 'NONE',  ( 2.500000000000000000, 2.357898499370431722, -2.818925648462311528E-15 ) ) ;
#1983 = ORIENTED_EDGE ( 'NONE', *, *, #11069, .T. ) ;
#1984 = CARTESIAN_POINT ( 'NONE',  ( 0.2500000000000002220, 4.898587196589412829E-16, -4.000000000000000000 ) ) ;
#1985 = ORIENTED_EDGE ( 'NONE', *, *, #3573, .T. ) ;
#1986 = DIRECTION ( 'NONE',  ( 1.350636282998972974E-14, 0.000000000000000000, -1.000000000000000000 ) ) ;
#1987 = DIRECTION ( 'NONE',  ( 1.000000000000000000, 0.000000000000000000, 0.000000000000000000 ) ) ;
#1988 = ORIENTED_EDGE ( 'NONE', *, *, #19088, .F. ) ;
#1989 = PRESENTATION_STYLE_ASSIGNMENT (( #1637 ) ) ;
#1990 = CARTESIAN_POINT ( 'NONE',  ( 123.7141469857648559, -1093.380023028672440, -32.17346063704734860 ) ) ;
#1991 = DIRECTION ( 'NONE',  ( -0.000000000000000000, -0.000000000000000000, 1.000000000000000000 ) ) ;
#1992 = DIRECTION ( 'NONE',  ( 0.000000000000000000, -1.000000000000000000, -5.286776307738891306E-15 ) ) ;
#1993 = DIRECTION ( 'NONE',  ( -0.5114233182937452105, 0.4883095222350190001, 0.7071067811865631159 ) ) ;
#1994 = CARTESIAN_POINT ( 'NONE',  ( 7.500000000000000000, -4.330127018922199866, -7.422398894150035176 ) ) ;
#1995 = CARTESIAN_POINT ( 'NONE',  ( 0.000000000000000000, 0.000000000000000000, 100.0000000000000000 ) ) ;
#1996 = VERTEX_POINT ( 'NONE', #23608 ) ;
#1997 = DIRECTION ( 'NONE',  ( 0.000000000000000000, 0.000000000000000000, 1.000000000000000000 ) ) ;
#1999 = LINE ( 'NONE', #18545, #5388 ) ;
#1998 =( REPRESENTATION_RELATIONSHIP ('NONE','NONE', #10127, #6236 ) REPRESENTATION_RELATIONSHIP_WITH_TRANSFORMATION ( #15144 )SHAPE_REPRESENTATION_RELATIONSHIP( ) );
#2000 = ORIENTED_EDGE ( 'NONE', *, *, #13822, .F. ) ;
#2001 = AXIS2_PLACEMENT_3D ( 'NONE', #14523, #21858, #3611 ) ;
#2002 = EDGE_CURVE ( 'NONE', #18582, #6504, #3774, .T. ) ;
#2003 = FACE_OUTER_BOUND ( 'NONE', #15550, .T. ) ;
#2004 = FACE_OUTER_BOUND ( 'NONE', #4666, .T. ) ;
#2005 = DIRECTION ( 'NONE',  ( -1.000000000000000000, -2.775557561562891351E-17, 0.000000000000000000 ) ) ;
#2006 = ORIENTED_EDGE ( 'NONE', *, *, #20259, .F. ) ;
#2007 = DIRECTION ( 'NONE',  ( 0.000000000000000000, -3.469446951953613794E-15, -1.000000000000000000 ) ) ;
#2008 = LINE ( 'NONE', #1661, #18975 ) ;
#2009 = CARTESIAN_POINT ( 'NONE',  ( -8.737863883542575039, -5.036189803708990276, 200.0000119999999697 ) ) ;
#2010 = ORIENTED_EDGE ( 'NONE', *, *, #19334, .T. ) ;
#2011 = DIRECTION ( 'NONE',  ( 0.000000000000000000, -1.000000000000000000, 0.000000000000000000 ) ) ;
#2012 = CARTESIAN_POINT ( 'NONE',  ( -136.6960319176257883, -1073.069888270695401, 28.34183984639752651 ) ) ;
#2013 = CARTESIAN_POINT ( 'NONE',  ( -77.72886158240795851, -117.3074641843678876, 90.00000000000000000 ) ) ;
#2014 = ORIENTED_EDGE ( 'NONE', *, *, #13472, .F. ) ;
#2015 = CARTESIAN_POINT ( 'NONE',  ( 100.0000000000000000, 249.9999999999999716, 125.0000000000000284 ) ) ;
#2016 = VECTOR ( 'NONE', #23551, 1000.000000000000000 ) ;
#2017 = CARTESIAN_POINT ( 'NONE',  ( -56.99999999999995737, 1.586603881823895016E-29, 4.235035081596970394E-15 ) ) ;
#2018 = DIRECTION ( 'NONE',  ( 1.000000000000000000, 0.000000000000000000, 0.000000000000000000 ) ) ;
#2019 = CARTESIAN_POINT ( 'NONE',  ( -40.00000000000000000, 100.0000000000000000, 125.0000000000000000 ) ) ;
#2020 = EDGE_LOOP ( 'NONE', ( #17265, #10424, #23573, #20503 ) ) ;
#2021 = VERTEX_POINT ( 'NONE', #18282 ) ;
#2022 = DIRECTION ( 'NONE',  ( -1.000000000000000000, 3.495664435217746987E-15, 0.000000000000000000 ) ) ;
#2023 = EDGE_CURVE ( 'NONE', #16783, #7859, #14353, .T. ) ;
#2024 = PRODUCT_DEFINITION_CONTEXT ( 'detailed design', #19698, 'design' ) ;
#2025 = EDGE_CURVE ( 'NONE', #22322, #15324, #12552, .T. ) ;
#2026 = AXIS2_PLACEMENT_3D ( 'NONE', #8177, #8284, #19258 ) ;
#2027 = VERTEX_POINT ( 'NONE', #3439 ) ;
#2028 = DIRECTION ( 'NONE',  ( 0.000000000000000000, 0.000000000000000000, 1.000000000000000000 ) ) ;
#2029 = FACE_OUTER_BOUND ( 'NONE', #11694, .T. ) ;
#2030 = ORIENTED_EDGE ( 'NONE', *, *, #6055, .F. ) ;
#2031 = LINE ( 'NONE', #10783, #1383 ) ;
#2032 = EDGE_CURVE ( 'NONE', #17746, #2765, #11464, .T. ) ;
#2033 = EDGE_CURVE ( 'NONE', #11764, #2480, #23769, .T. ) ;
#2034 = VERTEX_POINT ( 'NONE', #7174 ) ;
#2035 = FACE_OUTER_BOUND ( 'NONE', #3165, .T. ) ;
#2036 = DIRECTION ( 'NONE',  ( 0.000000000000000000, 1.000000000000000000, 0.000000000000000000 ) ) ;
#2037 = VERTEX_POINT ( 'NONE', #10722 ) ;
#2038 = DIRECTION ( 'NONE',  ( 0.000000000000000000, 0.000000000000000000, 1.000000000000000000 ) ) ;
#2039 = VECTOR ( 'NONE', #10467, 1000.000000000000000 ) ;
#2040 = ADVANCED_FACE ( 'NONE', ( #23719 ), #16138, .T. ) ;
#2041 = FACE_OUTER_BOUND ( 'NONE', #5191, .T. ) ;
#2042 = TOROIDAL_SURFACE ( 'NONE', #23274, 20.30000000000000071, 0.3000000000000059841 ) ;
#2043 = DIRECTION ( 'NONE',  ( -0.000000000000000000, -0.000000000000000000, 1.000000000000000000 ) ) ;
#2044 = VECTOR ( 'NONE', #18359, 1000.000000000000000 ) ;
#2045 = DIRECTION ( 'NONE',  ( 0.000000000000000000, 2.618450529776313049E-15, 1.000000000000000000 ) ) ;
#2046 = CYLINDRICAL_SURFACE ( 'NONE', #9224, 145.0000000000000284 ) ;
#2047 = EDGE_LOOP ( 'NONE', ( #14884, #22108, #1224, #7071 ) ) ;
#2048 = CARTESIAN_POINT ( 'NONE',  ( 2.500000000000000000, 2.357898499370433054, -1.951563910473907981E-15 ) ) ;
#2049 = DIRECTION ( 'NONE',  ( 0.000000000000000000, 0.000000000000000000, 1.000000000000000000 ) ) ;
#2050 =( NAMED_UNIT ( * ) SI_UNIT ( $, .STERADIAN. ) SOLID_ANGLE_UNIT ( ) );
#2052 = EDGE_LOOP ( 'NONE', ( #2396, #7471, #17213, #12512 ) ) ;
#2051 = ORIENTED_EDGE ( 'NONE', *, *, #11144, .T. ) ;
#2053 = DIRECTION ( 'NONE',  ( 1.000000000000000000, 0.000000000000000000, 0.000000000000000000 ) ) ;
#2054 = CARTESIAN_POINT ( 'NONE',  ( -136.5237489982507100, -1073.391313005787424, -31.99339931332765374 ) ) ;
#2055 = CARTESIAN_POINT ( 'NONE',  ( 45.24999999999994316, 100.0000000000000000, 150.2000000000009550 ) ) ;
#2056 = ORIENTED_EDGE ( 'NONE', *, *, #3809, .T. ) ;
#2057 = AXIS2_PLACEMENT_3D ( 'NONE', #14966, #22065, #4060 ) ;
#2058 = CARTESIAN_POINT ( 'NONE',  ( -7.922281120364393914, 4.573931137438271399, -8.047472243342930653 ) ) ;
#2059 = AXIS2_PLACEMENT_3D ( 'NONE', #3328, #21587, #21697 ) ;
#2060 = ORIENTED_EDGE ( 'NONE', *, *, #9485, .F. ) ;
#2061 = EDGE_CURVE ( 'NONE', #23382, #13229, #21904, .T. ) ;
#2062 = DIRECTION ( 'NONE',  ( 0.000000000000000000, 0.000000000000000000, -1.000000000000000000 ) ) ;
#2063 = ADVANCED_FACE ( 'NONE', ( #297 ), #541, .F. ) ;
#2065 = EDGE_LOOP ( 'NONE', ( #6823, #9129 ) ) ;
#2064 = B_SPLINE_CURVE_WITH_KNOTS ( 'NONE', 3,
 ( #4053, #18658, #2494, #22291, #9881, #2125 ),
 .UNSPECIFIED., .F., .F.,
 ( 4, 2, 4 ),
 ( 0.002365888236228001588, 0.003551327329835089319, 0.004736766423442177049 ),
 .UNSPECIFIED. ) ;
#2066 = EDGE_CURVE ( 'NONE', #3824, #11584, #7536, .T. ) ;
#2067 = DIRECTION ( 'NONE',  ( 1.000000000000000000, 0.000000000000000000, 0.000000000000000000 ) ) ;
#2068 = SURFACE_STYLE_USAGE ( .BOTH. , #15261 ) ;
#2069 = VERTEX_POINT ( 'NONE', #18627 ) ;
#2070 = EDGE_CURVE ( 'NONE', #1763, #22378, #13506, .T. ) ;
#2071 = ADVANCED_FACE ( 'NONE', ( #7655 ), #15697, .F. ) ;
#2072 = DIRECTION ( 'NONE',  ( 0.000000000000000000, -0.5000000000000009992, -0.8660254037844380415 ) ) ;
#2073 = ADVANCED_BREP_SHAPE_REPRESENTATION ( '', ( #20279, #11210 ), #9278 ) ;
#2074 = ORIENTED_EDGE ( 'NONE', *, *, #31, .T. ) ;
#2075 = EDGE_CURVE ( 'NONE', #21835, #17715, #16831, .T. ) ;
#2076 = CARTESIAN_POINT ( 'NONE',  ( -128.7717867965311598, 86.27213916325780474, 32.00444854364504010 ) ) ;
#2077 = CARTESIAN_POINT ( 'NONE',  ( -160.0000000000000000, 0.000000000000000000, 100.0000000000000000 ) ) ;
#2078 = CARTESIAN_POINT ( 'NONE',  ( 4.000000000000000000, -1.700175430507292473, -3.320327275037661785 ) ) ;
#2079 = CIRCLE ( 'NONE', #5950, 2.500000000000002220 ) ;
#2080 = CARTESIAN_POINT ( 'NONE',  ( 112.7436279071538792, -91.18044947428829516, 90.00000000000000000 ) ) ;
#2081 = ORIENTED_EDGE ( 'NONE', *, *, #10315, .T. ) ;
#2082 = CARTESIAN_POINT ( 'NONE',  ( 24.99999999999998224, -1000.000000000000000, 138.9999999999999716 ) ) ;
#2083 =( LENGTH_UNIT ( ) NAMED_UNIT ( * ) SI_UNIT ( .MILLI., .METRE. ) );
#2084 = CIRCLE ( 'NONE', #19047, 4.057500000000000107 ) ;
#2085 = ORIENTED_EDGE ( 'NONE', *, *, #460, .T. ) ;
#2086 =( NAMED_UNIT ( * ) SI_UNIT ( $, .STERADIAN. ) SOLID_ANGLE_UNIT ( ) );
#2087 = CARTESIAN_POINT ( 'NONE',  ( -7.703920929261754758, -4.447860822324869901, -7.917989418073284824 ) ) ;
#2088 = CARTESIAN_POINT ( 'NONE',  ( -282.2000000000007276, 75.00000000000099476, -90.00000000000000000 ) ) ;
#2089 = CARTESIAN_POINT ( 'NONE',  ( 5.000000000000000888, 0.000000000000000000, 0.000000000000000000 ) ) ;
#2090 = DIRECTION ( 'NONE',  ( 0.000000000000000000, 0.000000000000000000, -1.000000000000000000 ) ) ;
#2091 = AXIS2_PLACEMENT_3D ( 'NONE', #15406, #19116, #6576 ) ;
#2092 = VECTOR ( 'NONE', #1739, 1000.000000000000000 ) ;
#2093 = DIRECTION ( 'NONE',  ( -1.110223024625155594E-14, 0.000000000000000000, -1.000000000000000000 ) ) ;
#2094 = CARTESIAN_POINT ( 'NONE',  ( 135.4018704341550290, 51.87806360044960030, -2.775557561562891351E-14 ) ) ;
#2095 = EDGE_LOOP ( 'NONE', ( #19025, #1291, #11024, #6887 ) ) ;
#2096 = CARTESIAN_POINT ( 'NONE',  ( -6.482064212728105623, -975.7995837828526646, 145.0000119999999697 ) ) ;
#2097 = ORIENTED_EDGE ( 'NONE', *, *, #6210, .F. ) ;
#2098 = CARTESIAN_POINT ( 'NONE',  ( -93.00000000000000000, 3.053113317719180486E-13, 129.9038105676659711 ) ) ;
#2099 = FACE_BOUND ( 'NONE', #3228, .T. ) ;
#2100 = ADVANCED_FACE ( 'NONE', ( #7902 ), #18879, .F. ) ;
#2101 = EDGE_CURVE ( 'NONE', #2069, #12336, #14538, .T. ) ;
#2102 = EDGE_CURVE ( 'NONE', #10287, #52, #11208, .T. ) ;
#2103 = LINE ( 'NONE', #22396, #1327 ) ;
#2104 = ORIENTED_EDGE ( 'NONE', *, *, #19525, .F. ) ;
#2105 = CARTESIAN_POINT ( 'NONE',  ( -3.000000000000002665, 0.000000000000000000, -23.97500000000000142 ) ) ;
#2106 = DIRECTION ( 'NONE',  ( -1.000000000000000000, -0.000000000000000000, -0.000000000000000000 ) ) ;
#2107 = DIRECTION ( 'NONE',  ( -0.000000000000000000, -1.000000000000000000, 3.495664435217746987E-15 ) ) ;
#2108 = CARTESIAN_POINT ( 'NONE',  ( 2.500000000000000000, 2.500728763858895382E-16, -2.041999999999999815 ) ) ;
#2109 = PLANE ( 'NONE',  #11547 ) ;
#2110 = DIRECTION ( 'NONE',  ( 0.000000000000000000, 0.000000000000000000, -1.000000000000000000 ) ) ;
#2111 = CARTESIAN_POINT ( 'NONE',  ( 1.500000000000001332, 7.960204194457796463E-16, -6.500000000000000888 ) ) ;
#2112 = VECTOR ( 'NONE', #4939, 1000.000000000000000 ) ;
#2113 = VERTEX_POINT ( 'NONE', #5610 ) ;
#2114 = LINE ( 'NONE', #15436, #11916 ) ;
#2115 = DIRECTION ( 'NONE',  ( 1.000000000000000000, -0.000000000000000000, 6.982962677686266711E-15 ) ) ;
#2116 = ORIENTED_EDGE ( 'NONE', *, *, #20811, .F. ) ;
#2117 = CIRCLE ( 'NONE', #16041, 2.650000000000041211 ) ;
#2118 = VERTEX_POINT ( 'NONE', #22257 ) ;
#2119 = CLOSED_SHELL ( 'NONE', ( #11014, #8439, #10072, #10910, #10265, #5080, #12865, #9217, #22299, #4330, #4702, #12929, #9483, #15970, #10638, #16706, #17876, #12809, #18580, #3085, #19020, #1797, #21300, #15713, #21013, #4070, #20526, #23261, #1648, #2484, #22952, #22307, #20455, #20983, #11680, #20762, #3343, #6062, #12723, #11249, #6402, #468, #19361, #22412, #9019, #23041 ) ) ;
#2120 = CYLINDRICAL_SURFACE ( 'NONE', #2712, 20.00000000000000000 ) ;
#2121 = DIRECTION ( 'NONE',  ( 0.000000000000000000, 0.000000000000000000, 1.000000000000000000 ) ) ;
#2122 = LINE ( 'NONE', #330, #4808 ) ;
#2123 = ORIENTED_EDGE ( 'NONE', *, *, #21274, .F. ) ;
#2124 = AXIS2_PLACEMENT_3D ( 'NONE', #339, #11607, #2613 ) ;
#2125 = CARTESIAN_POINT ( 'NONE',  ( -4.000000000000000000, -2.309401076758515803, -0.4999999999999995559 ) ) ;
#2126 = LINE ( 'NONE', #5879, #22069 ) ;
#2127 = CARTESIAN_POINT ( 'NONE',  ( 146.0000000000001990, -210.0000000000003411, -27.94499999999356632 ) ) ;
#2128 = EDGE_LOOP ( 'NONE', ( #13996, #8253, #645, #9491 ) ) ;
#2129 = PLANE ( 'NONE',  #2515 ) ;
#2130 = CARTESIAN_POINT ( 'NONE',  ( -102.3500000000000227, -29.99999999999998579, 3.000000000000000000 ) ) ;
#2131 = CARTESIAN_POINT ( 'NONE',  ( -1.240299975428113101E-15, -4.647091401871173311, -3.572172305156514849 ) ) ;
#2132 = ORIENTED_EDGE ( 'NONE', *, *, #5885, .F. ) ;
#2133 = DIRECTION ( 'NONE',  ( 0.000000000000000000, -1.000000000000000000, 0.000000000000000000 ) ) ;
#2134 = AXIS2_PLACEMENT_3D ( 'NONE', #1714, #20186, #5705 ) ;
#2135 = PRODUCT_CONTEXT ( 'NONE', #11093, 'mechanical' ) ;
#2136 = CARTESIAN_POINT ( 'NONE',  ( -285.2000000000010118, 9.892604858775022387E-13, 0.000000000000000000 ) ) ;
#2137 = CARTESIAN_POINT ( 'NONE',  ( -146.4450000000000784, -204.4690652294807194, 30.00000000000641975 ) ) ;
#2138 = DIRECTION ( 'NONE',  ( 0.000000000000000000, 0.000000000000000000, 1.000000000000000000 ) ) ;
#2139 = ORIENTED_EDGE ( 'NONE', *, *, #12338, .F. ) ;
#2140 = ORIENTED_EDGE ( 'NONE', *, *, #17933, .F. ) ;
#2141 = DIRECTION ( 'NONE',  ( 0.000000000000000000, 0.000000000000000000, 1.000000000000000000 ) ) ;
#2142 = TOROIDAL_SURFACE ( 'NONE', #987, 2.700000000000000622, 0.2000000000000000111 ) ;
#2143 = DIRECTION ( 'NONE',  ( -0.000000000000000000, -0.000000000000000000, 1.000000000000000000 ) ) ;
#2144 = ORIENTED_EDGE ( 'NONE', *, *, #17878, .T. ) ;
#2145 = CARTESIAN_POINT ( 'NONE',  ( 0.000000000000000000, 0.000000000000000000, 155.0000000000000284 ) ) ;
#2146 = DIRECTION ( 'NONE',  ( 1.751623080406021339E-46, 3.469446951953613794E-15, 1.000000000000000000 ) ) ;
#2147 = VERTEX_POINT ( 'NONE', #4281 ) ;
#2148 = DIRECTION ( 'NONE',  ( -0.000000000000000000, 1.000000000000000000, -0.000000000000000000 ) ) ;
#2149 = ADVANCED_FACE ( 'NONE', ( #9603 ), #11320, .F. ) ;
#2150 = VERTEX_POINT ( 'NONE', #22389 ) ;
#2151 = AXIS2_PLACEMENT_3D ( 'NONE', #13145, #20452, #18988 ) ;
#2152 = CYLINDRICAL_SURFACE ( 'NONE', #19096, 2.649999999999999467 ) ;
#2153 = DIRECTION ( 'NONE',  ( 0.000000000000000000, 1.000000000000000000, -1.295896757998781966E-15 ) ) ;
#2154 = ORIENTED_EDGE ( 'NONE', *, *, #13234, .T. ) ;
#2155 = ORIENTED_EDGE ( 'NONE', *, *, #11016, .F. ) ;
#2156 = CARTESIAN_POINT ( 'NONE',  ( -129.0286178947080771, 85.88727694560768100, -31.52881987646414430 ) ) ;
#2157 = EDGE_CURVE ( 'NONE', #11764, #22779, #3251, .T. ) ;
#2158 = CARTESIAN_POINT ( 'NONE',  ( -280.4357574145959120, 272.4730547946946331, -147.3059783239180547 ) ) ;
#2159 = AXIS2_PLACEMENT_3D ( 'NONE', #16619, #18062, #16480 ) ;
#2160 = DIRECTION ( 'NONE',  ( -0.000000000000000000, -0.000000000000000000, 1.000000000000000000 ) ) ;
#2161 = EDGE_CURVE ( 'NONE', #11272, #13966, #5851, .T. ) ;
#2162 = CARTESIAN_POINT ( 'NONE',  ( 155.0000000000000284, -500.0000000000000000, -32.64999999999995595 ) ) ;
#2163 = DIRECTION ( 'NONE',  ( -1.000000000000000000, 0.000000000000000000, -0.000000000000000000 ) ) ;
#2164 = DIRECTION ( 'NONE',  ( -0.8090169943749507819, 0.5877852522924686962, 0.000000000000000000 ) ) ;
#2165 = DIRECTION ( 'NONE',  ( 1.000000000000000000, 0.000000000000000000, 0.000000000000000000 ) ) ;
#2166 = EDGE_LOOP ( 'NONE', ( #7941, #3894, #10485, #2701 ) ) ;
#2167 = FACE_OUTER_BOUND ( 'NONE', #8850, .T. ) ;
#2168 = CARTESIAN_POINT ( 'NONE',  ( 45.00000000000004974, -52.79999999999966320, 52.65000000000018332 ) ) ;
#2169 = SHAPE_REPRESENTATION_RELATIONSHIP ( 'NONE' , 'NONE' ,  #14711, #2073 ) ;
#2170 = EDGE_CURVE ( 'NONE', #19782, #15625, #13019, .T. ) ;
#2172 = ORIENTED_EDGE ( 'NONE', *, *, #16834, .T. ) ;
#2171 = VERTEX_POINT ( 'NONE', #2211 ) ;
#2173 = CARTESIAN_POINT ( 'NONE',  ( 232.0000000000000284, -489.9999999999998863, 57.00000000000002132 ) ) ;
#2174 = AXIS2_PLACEMENT_3D ( 'NONE', #15138, #20655, #4110 ) ;
#2175 = CARTESIAN_POINT ( 'NONE',  ( 280.8708543776411943, 271.0140793454688151, -149.1822575857424056 ) ) ;
#2176 = ORIENTED_EDGE ( 'NONE', *, *, #14759, .T. ) ;
#2177 = CARTESIAN_POINT ( 'NONE',  ( -134.8603954219443608, -1076.404761192049591, 28.34264858295328438 ) ) ;
#2178 = VERTEX_POINT ( 'NONE', #13376 ) ;
#2179 = CARTESIAN_POINT ( 'NONE',  ( 281.3488036478620415, 272.8335297745772436, -145.2489140339769449 ) ) ;
#2180 = VERTEX_POINT ( 'NONE', #18526 ) ;
#2181 = DIRECTION ( 'NONE',  ( 0.000000000000000000, -0.4999999999999993339, 0.8660254037844390407 ) ) ;
#2182 = CARTESIAN_POINT ( 'NONE',  ( -100.0000000000001137, -132.1999999999999602, 152.4000000000014268 ) ) ;
#2183 = AXIS2_PLACEMENT_3D ( 'NONE', #6288, #21018, #15246 ) ;
#2184 = ITEM_DEFINED_TRANSFORMATION ( 'NONE', 'NONE', #18143,  #11210 ) ;
#2185 = ORIENTED_EDGE ( 'NONE', *, *, #4517, .F. ) ;
#2186 =( BOUNDED_SURFACE ( )  B_SPLINE_SURFACE ( 3, 2, ( 
 ( #4668, #8533, #12082 ),
 ( #4419, #4895, #21206 ),
 ( #6822, #15779, #2598 ),
 ( #19611, #21431, #3078 ),
 ( #2734, #13757, #15554 ),
 ( #21079, #14220, #23363 ) ),
 .UNSPECIFIED., .F., .F., .F. ) 
 B_SPLINE_SURFACE_WITH_KNOTS ( ( 4, 2, 4 ),
 ( 3, 3 ),
 ( 0.02027752710269158445, 0.02273781595091097299, 0.02519810479913036153 ),
 ( 0.000000000000000000, 1.000000000000000000 ),
 .UNSPECIFIED. ) 
 GEOMETRIC_REPRESENTATION_ITEM ( )  RATIONAL_B_SPLINE_SURFACE ( (
 ( 1.000000000000000000, 0.8047781431712808242, 1.000000000000000000),
 ( 1.000000000000000000, 0.8123773247083928561, 1.000000000000000000),
 ( 1.000000000000000000, 0.8190670192154906326, 1.000000000000000000),
 ( 1.000000000000000000, 0.8192353552912178261, 1.000000000000000000),
 ( 1.000000000000000000, 0.8126132098226825917, 1.000000000000000000),
 ( 1.000000000000000000, 0.8047712465856394770, 1.000000000000000000) ) ) 
 REPRESENTATION_ITEM ( '' )  SURFACE ( )  );
#2187 = CYLINDRICAL_SURFACE ( 'NONE', #236, 7.500000000000007105 ) ;
#2188 = VERTEX_POINT ( 'NONE', #20687 ) ;
#2189 = VECTOR ( 'NONE', #10752, 1000.000000000000000 ) ;
#2190 = CARTESIAN_POINT ( 'NONE',  ( -128.2758413234849399, 87.00805048166478173, 27.56549073392523397 ) ) ;
#2191 = PLANE ( 'NONE',  #14998 ) ;
#2192 = DIRECTION ( 'NONE',  ( 0.000000000000000000, 1.177509268541832635E-16, -1.000000000000000000 ) ) ;
#2193 = EDGE_LOOP ( 'NONE', ( #20883, #8607 ) ) ;
#2194 = CARTESIAN_POINT ( 'NONE',  ( -281.2440776823445390, 268.3679143846943589, -147.1132285165672045 ) ) ;
#2195 = SURFACE_SIDE_STYLE ('',( #4502 ) ) ;
#2196 = EDGE_CURVE ( 'NONE', #14422, #19693, #11391, .T. ) ;
#2197 = ADVANCED_FACE ( 'NONE', ( #4147 ), #11560, .F. ) ;
#2198 = ORIENTED_EDGE ( 'NONE', *, *, #16661, .T. ) ;
#2199 = CARTESIAN_POINT ( 'NONE',  ( -194.3969595146226084, 487.6831165126316137, 0.000000000000000000 ) ) ;
#2200 = FACE_OUTER_BOUND ( 'NONE', #20512, .T. ) ;
#2201 = CARTESIAN_POINT ( 'NONE',  ( 0.000000000000000000, 0.000000000000000000, 100.0000000000000000 ) ) ;
#2202 = AXIS2_PLACEMENT_3D ( 'NONE', #14375, #18086, #9030 ) ;
#2203 = EDGE_CURVE ( 'NONE', #13113, #20328, #942, .T. ) ;
#2204 = DIRECTION ( 'NONE',  ( -1.000000000000000000, -0.000000000000000000, -0.000000000000000000 ) ) ;
#2205 = DIRECTION ( 'NONE',  ( -0.000000000000000000, -0.000000000000000000, -1.000000000000000000 ) ) ;
#2206 = AXIS2_PLACEMENT_3D ( 'NONE', #13977, #1245, #21179 ) ;
#2207 = ORIENTED_EDGE ( 'NONE', *, *, #5582, .T. ) ;
#2208 = EDGE_CURVE ( 'NONE', #17463, #13673, #4416, .T. ) ;
#2209 = CIRCLE ( 'NONE', #15734, 2.500000000000000888 ) ;
#2210 = CARTESIAN_POINT ( 'NONE',  ( -281.4928932188134922, 5.173457871231059415E-13, -150.2000000000008981 ) ) ;
#2211 = CARTESIAN_POINT ( 'NONE',  ( -282.2000000000006708, 90.00000000000102318, -37.64999999999999147 ) ) ;
#2212 = CARTESIAN_POINT ( 'NONE',  ( 123.9854850298566618, -1093.019475613609529, 32.37408494914630808 ) ) ;
#2213 = VERTEX_POINT ( 'NONE', #4513 ) ;
#2214 = CARTESIAN_POINT ( 'NONE',  ( -3.272451888078324433, -975.1611521969856540, 145.0000119999999697 ) ) ;
#2215 = ORIENTED_EDGE ( 'NONE', *, *, #19914, .T. ) ;
#2216 = CARTESIAN_POINT ( 'NONE',  ( -282.2000000000007276, 75.00000000000099476, -90.00000000000000000 ) ) ;
#2217 = DIRECTION ( 'NONE',  ( -1.000000000000000000, -0.000000000000000000, -0.000000000000000000 ) ) ;
#2218 = DIRECTION ( 'NONE',  ( -0.000000000000000000, 0.7071067811865485719, 0.7071067811865465735 ) ) ;
#2219 = ORIENTED_EDGE ( 'NONE', *, *, #1073, .T. ) ;
#2220 = AXIS2_PLACEMENT_3D ( 'NONE', #8767, #1502, #23485 ) ;
#2221 = CARTESIAN_POINT ( 'NONE',  ( -1.500000000000000000, 11.99999999999999822, 200.2421591959677016 ) ) ;
#2222 = DIRECTION ( 'NONE',  ( -0.000000000000000000, 0.4999999999999979461, -0.8660254037844397068 ) ) ;
#2223 = CARTESIAN_POINT ( 'NONE',  ( -155.0000000000000284, 0.000000000000000000, -90.00000000000000000 ) ) ;
#2224 = DIRECTION ( 'NONE',  ( -3.469446951953614682E-16, 1.000000000000000000, -3.483493295888648978E-15 ) ) ;
#2225 = ADVANCED_FACE ( 'NONE', ( #15529 ), #14083, .F. ) ;
#2226 = AXIS2_PLACEMENT_3D ( 'NONE', #21390, #8489, #4732 ) ;
#2227 = DIRECTION ( 'NONE',  ( -1.000000000000000000, -0.000000000000000000, -0.000000000000000000 ) ) ;
#2228 = CIRCLE ( 'NONE', #5325, 155.0000000000000284 ) ;
#2229 = DIRECTION ( 'NONE',  ( 1.110223024625155594E-14, 0.000000000000000000, -1.000000000000000000 ) ) ;
#2230 = VECTOR ( 'NONE', #5125, 1000.000000000000000 ) ;
#2231 = FACE_OUTER_BOUND ( 'NONE', #16287, .T. ) ;
#2232 = AXIS2_PLACEMENT_3D ( 'NONE', #15906, #3082, #23243 ) ;
#2233 = ORIENTED_EDGE ( 'NONE', *, *, #19149, .T. ) ;
#2234 = CARTESIAN_POINT ( 'NONE',  ( -34.75000000000003553, 100.0000000000000000, 150.2000000000009550 ) ) ;
#2235 = FACE_OUTER_BOUND ( 'NONE', #21609, .T. ) ;
#2236 = ORIENTED_EDGE ( 'NONE', *, *, #17314, .F. ) ;
#2237 = ORIENTED_EDGE ( 'NONE', *, *, #9220, .T. ) ;
#2238 = FACE_BOUND ( 'NONE', #22062, .T. ) ;
#2239 = DIRECTION ( 'NONE',  ( 0.000000000000000000, 0.000000000000000000, 1.000000000000000000 ) ) ;
#2240 = ADVANCED_FACE ( 'NONE', ( #998, #21301 ), #13978, .F. ) ;
#2241 = EDGE_CURVE ( 'NONE', #13509, #22474, #19838, .T. ) ;
#2242 = CARTESIAN_POINT ( 'NONE',  ( -285.2000000000000455, 267.7999999999999545, 146.4928932188134354 ) ) ;
#2243 = CIRCLE ( 'NONE', #5404, 2.500000000000002220 ) ;
#2244 = EDGE_LOOP ( 'NONE', ( #17085, #2250, #21077, #7054 ) ) ;
#2245 = AXIS2_PLACEMENT_3D ( 'NONE', #14370, #21589, #20895 ) ;
#2246 = DIRECTION ( 'NONE',  ( 0.000000000000000000, -1.000000000000000000, 0.000000000000000000 ) ) ;
#2247 = DIRECTION ( 'NONE',  ( 1.000000000000000000, 0.000000000000000000, 0.000000000000000000 ) ) ;
#2248 = AXIS2_PLACEMENT_3D ( 'NONE', #11280, #20061, #7381 ) ;
#2249 = CARTESIAN_POINT ( 'NONE',  ( -285.2000000000010687, -19.99999999999898392, 102.3500000000000227 ) ) ;
#2250 = ORIENTED_EDGE ( 'NONE', *, *, #14976, .F. ) ;
#2251 = CARTESIAN_POINT ( 'NONE',  ( 281.4928932188133217, 267.7999999999999545, 150.1999999999999886 ) ) ;
#2252 = DIRECTION ( 'NONE',  ( 0.000000000000000000, 0.000000000000000000, 1.000000000000000000 ) ) ;
#2253 = DIRECTION ( 'NONE',  ( 1.000000000000000000, 0.000000000000000000, 0.000000000000000000 ) ) ;
#2254 = ORIENTED_EDGE ( 'NONE', *, *, #5482, .F. ) ;
#2255 = LINE ( 'NONE', #17249, #15393 ) ;
#2256 = SHAPE_DEFINITION_REPRESENTATION ( #7091, #9771 ) ;
#2257 = FACE_BOUND ( 'NONE', #15612, .T. ) ;
#2258 = PLANE ( 'NONE',  #4571 ) ;
#2259 = DIRECTION ( 'NONE',  ( -0.000000000000000000, 0.8660254037844398178, 0.4999999999999980571 ) ) ;
#2260 = ORIENTED_EDGE ( 'NONE', *, *, #16101, .T. ) ;
#2261 = CIRCLE ( 'NONE', #350, 2.650000000000041211 ) ;
#2262 = VERTEX_POINT ( 'NONE', #23100 ) ;
#2263 = AXIS2_PLACEMENT_3D ( 'NONE', #3156, #11909, #19217 ) ;
#2264 = AXIS2_PLACEMENT_3D ( 'NONE', #806, #2604, #15082 ) ;
#2265 = CARTESIAN_POINT ( 'NONE',  ( 3.000000000000001776, 24.69999999999999929, 0.000000000000000000 ) ) ;
#2266 = CIRCLE ( 'NONE', #12366, 4.000000000000000000 ) ;
#2267 = DIRECTION ( 'NONE',  ( 1.350636282998972974E-14, 0.000000000000000000, -1.000000000000000000 ) ) ;
#2268 = MECHANICAL_DESIGN_GEOMETRIC_PRESENTATION_REPRESENTATION (  '', ( #13888 ), #17346 ) ;
#2269 = CIRCLE ( 'NONE', #4207, 5.249999999999949374 ) ;
#2270 = EDGE_CURVE ( 'NONE', #15596, #21835, #19465, .T. ) ;
#2271 = PRODUCT_DEFINITION_CONTEXT ( 'detailed design', #7866, 'design' ) ;
#2272 =( REPRESENTATION_RELATIONSHIP ('NONE','NONE', #10127, #4815 ) REPRESENTATION_RELATIONSHIP_WITH_TRANSFORMATION ( #20984 )SHAPE_REPRESENTATION_RELATIONSHIP( ) );
#2273 = ORIENTED_EDGE ( 'NONE', *, *, #5882, .T. ) ;
#2274 = CARTESIAN_POINT ( 'NONE',  ( -25.00000000000000000, 1.865214261513747767E-15, -138.9999999999999716 ) ) ;
#2275 = EDGE_CURVE ( 'NONE', #2992, #5216, #9439, .T. ) ;
#2276 = CARTESIAN_POINT ( 'NONE',  ( -90.00000000000000000, 3.053113317719180486E-13, 129.9038105676659711 ) ) ;
#2277 = VECTOR ( 'NONE', #516, 1000.000000000000000 ) ;
#2278 = ORIENTED_EDGE ( 'NONE', *, *, #7743, .F. ) ;
#2279 = CARTESIAN_POINT ( 'NONE',  ( 4.000000000000000000, 0.000000000000000000, 0.000000000000000000 ) ) ;
#2280 = ORIENTED_EDGE ( 'NONE', *, *, #2696, .F. ) ;
#2282 = AXIS2_PLACEMENT_3D ( 'NONE', #9976, #11933, #2927 ) ;
#2281 = AXIS2_PLACEMENT_3D ( 'NONE', #19942, #18150, #8500 ) ;
#2284 = CARTESIAN_POINT ( 'NONE',  ( 72.64999999999999147, -87.33333333333332860, 145.0000000000000000 ) ) ;
#2283 = AXIS2_PLACEMENT_3D ( 'NONE', #6230, #5097, #15543 ) ;
#2285 = CIRCLE ( 'NONE', #16192, 145.0000000000000284 ) ;
#2287 = AXIS2_PLACEMENT_3D ( 'NONE', #23603, #7418, #3311 ) ;
#2286 = CARTESIAN_POINT ( 'NONE',  ( 2.500000000000002220, 0.000000000000000000, 0.000000000000000000 ) ) ;
#2288 = EDGE_LOOP ( 'NONE', ( #8770, #2316, #14048, #18273 ) ) ;
#2289 = ORIENTED_EDGE ( 'NONE', *, *, #7190, .T. ) ;
#2290 = CARTESIAN_POINT ( 'NONE',  ( -34.75000000000005684, 100.0000000000000000, -125.0000000000000000 ) ) ;
#2291 = VECTOR ( 'NONE', #8624, 1000.000000000000000 ) ;
#2292 = VECTOR ( 'NONE', #4806, 1000.000000000000000 ) ;
#2293 = CARTESIAN_POINT ( 'NONE',  ( 3.678949249685231848, 0.000000000000000000, 0.000000000000000000 ) ) ;
#2294 = CARTESIAN_POINT ( 'NONE',  ( 145.9999999999998010, -209.9999999999996874, 30.00000000000641620 ) ) ;
#2295 = CARTESIAN_POINT ( 'NONE',  ( -280.2906609804449545, 269.9854425596107603, -145.1255802622536351 ) ) ;
#2296 = CARTESIAN_POINT ( 'NONE',  ( 45.00000000000004974, -56.79999999999964899, 105.0000000000002132 ) ) ;
#2297 = CARTESIAN_POINT ( 'NONE',  ( 5.200000000000002842, 0.000000000000000000, 2.500000000000000444 ) ) ;
#2298 = CARTESIAN_POINT ( 'NONE',  ( -7.703011046602857601E-15, -132.2000000000000455, -146.4928932188134070 ) ) ;
#2299 = ORIENTED_EDGE ( 'NONE', *, *, #7009, .F. ) ;
#2300 = FACE_OUTER_BOUND ( 'NONE', #14406, .T. ) ;
#2301 = FACE_OUTER_BOUND ( 'NONE', #15644, .T. ) ;
#2302 = ADVANCED_FACE ( 'NONE', ( #11927 ), #6217, .F. ) ;
#2303 = ORIENTED_EDGE ( 'NONE', *, *, #4569, .F. ) ;
#2304 = EDGE_CURVE ( 'NONE', #22539, #22426, #16759, .T. ) ;
#2306 = AXIS2_PLACEMENT_3D ( 'NONE', #17479, #924, #6615 ) ;
#2305 = PRODUCT_DEFINITION_FORMATION_WITH_SPECIFIED_SOURCE ( 'ANY', '', #12733, .NOT_KNOWN. ) ;
#2307 = CARTESIAN_POINT ( 'NONE',  ( -136.1024116720897723, -1074.169801158669088, -32.42132972170178107 ) ) ;
#2308 = CARTESIAN_POINT ( 'NONE',  ( 280.9952621458755857, 270.4339272673397545, -149.5699028110927316 ) ) ;
#2309 = VECTOR ( 'NONE', #4239, 1000.000000000000000 ) ;
#2310 = ORIENTED_EDGE ( 'NONE', *, *, #6574, .F. ) ;
#2311 = EDGE_CURVE ( 'NONE', #2349, #5795, #6442, .T. ) ;
#2312 = FACE_BOUND ( 'NONE', #23205, .T. ) ;
#2313 = ORIENTED_EDGE ( 'NONE', *, *, #19119, .T. ) ;
#2314 = FACE_OUTER_BOUND ( 'NONE', #10322, .T. ) ;
#2315 = CIRCLE ( 'NONE', #14619, 2.499999999999998668 ) ;
#2316 = ORIENTED_EDGE ( 'NONE', *, *, #13829, .T. ) ;
#2317 = CYLINDRICAL_SURFACE ( 'NONE', #4211, 145.0000000000000284 ) ;
#2318 = EDGE_CURVE ( 'NONE', #16501, #13664, #5742, .T. ) ;
#2319 = CONTEXT_DEPENDENT_SHAPE_REPRESENTATION ( #13, #20900 ) ;
#2320 = VERTEX_POINT ( 'NONE', #10099 ) ;
#2321 = CARTESIAN_POINT ( 'NONE',  ( 2.500000000000000000, 2.253471898105738645E-15, 2.041999999999999815 ) ) ;
#2322 = PRODUCT_DEFINITION_FORMATION_WITH_SPECIFIED_SOURCE ( 'ANY', '', #3218, .NOT_KNOWN. ) ;
#2323 = VERTEX_POINT ( 'NONE', #21411 ) ;
#2324 = CARTESIAN_POINT ( 'NONE',  ( -24.99999999999998224, -1000.000000000000000, -145.0000060000000417 ) ) ;
#2325 = DIRECTION ( 'NONE',  ( 0.000000000000000000, -0.4999999999999991118, 0.8660254037844390407 ) ) ;
#2326 = VECTOR ( 'NONE', #14074, 1000.000000000000000 ) ;
#2327 = PLANE ( 'NONE',  #9596 ) ;
#2328 = FACE_OUTER_BOUND ( 'NONE', #10229, .T. ) ;
#2329 = ORIENTED_EDGE ( 'NONE', *, *, #19411, .T. ) ;
#2330 = CARTESIAN_POINT ( 'NONE',  ( -281.3405375976307710, 269.5502846751311949, 145.6212670861564504 ) ) ;
#2332 = ORIENTED_EDGE ( 'NONE', *, *, #9667, .F. ) ;
#2331 = ORIENTED_EDGE ( 'NONE', *, *, #11366, .F. ) ;
#2333 = DIRECTION ( 'NONE',  ( 6.982962677686266711E-15, 0.000000000000000000, -1.000000000000000000 ) ) ;
#2334 = CARTESIAN_POINT ( 'NONE',  ( 0.000000000000000000, 0.000000000000000000, 3.000000000000000000 ) ) ;
#2335 = CARTESIAN_POINT ( 'NONE',  ( 45.24999999999994316, 100.0000000000000000, 125.0000000000000000 ) ) ;
#2336 = LINE ( 'NONE', #9962, #8477 ) ;
#2337 = EDGE_CURVE ( 'NONE', #9953, #10712, #15398, .T. ) ;
#2338 = DIRECTION ( 'NONE',  ( -1.000000000000000000, 0.000000000000000000, 0.000000000000000000 ) ) ;
#2339 = EDGE_CURVE ( 'NONE', #6206, #13931, #4971, .T. ) ;
#2340 = VERTEX_POINT ( 'NONE', #17443 ) ;
#2341 = SHAPE_REPRESENTATION ( 'driver shaft', ( #11210 ), #22731 ) ;
#2342 = LINE ( 'NONE', #540, #13059 ) ;
#2343 = DIRECTION ( 'NONE',  ( 1.000000000000000000, 0.000000000000000000, 0.000000000000000000 ) ) ;
#2344 = CARTESIAN_POINT ( 'NONE',  ( 2.500000000000000000, -1.178949249685218303, -2.041999999999998039 ) ) ;
#2345 = ADVANCED_FACE ( 'NONE', ( #883, #8262, #2577 ), #9970, .T. ) ;
#2346 = VERTEX_POINT ( 'NONE', #19589 ) ;
#2347 = CARTESIAN_POINT ( 'NONE',  ( 5.000000000000000000, -3.513898075855361292, -2.028749999999995168 ) ) ;
#2348 = EDGE_CURVE ( 'NONE', #1928, #2426, #8066, .T. ) ;
#2349 = VERTEX_POINT ( 'NONE', #8027 ) ;
#2350 = DIRECTION ( 'NONE',  ( -0.000000000000000000, -0.000000000000000000, 1.000000000000000000 ) ) ;
#2351 = DIRECTION ( 'NONE',  ( -0.000000000000000000, 0.000000000000000000, 1.000000000000000000 ) ) ;
#2352 = ORIENTED_EDGE ( 'NONE', *, *, #2304, .F. ) ;
#2353 = CYLINDRICAL_SURFACE ( 'NONE', #129, 2.649999999999971934 ) ;
#2354 = EDGE_LOOP ( 'NONE', ( #7769, #2060 ) ) ;
#2355 = PLANE ( 'NONE',  #19619 ) ;
#2356 = DIRECTION ( 'NONE',  ( 1.000000000000000000, -0.000000000000000000, 0.000000000000000000 ) ) ;
#2357 = DIRECTION ( 'NONE',  ( 0.000000000000000000, -0.5000000000000009992, -0.8660254037844380415 ) ) ;
#2358 = EDGE_CURVE ( 'NONE', #18246, #16847, #12060, .T. ) ;
#2359 = CARTESIAN_POINT ( 'NONE',  ( 2.682243648011666703, 3.070208061305304881, -0.04852650426601266831 ) ) ;
#2360 = DIRECTION ( 'NONE',  ( -1.110223024625157172E-14, 0.000000000000000000, -1.000000000000000000 ) ) ;
#2361 = CARTESIAN_POINT ( 'NONE',  ( 160.0000000000000000, 1.959434878635765210E-14, 100.0000000000000000 ) ) ;
#2362 = FACE_OUTER_BOUND ( 'NONE', #23526, .T. ) ;
#2363 = B_SPLINE_CURVE_WITH_KNOTS ( 'NONE', 3,
 ( #13285, #22170, #20352, #7446, #210, #11598, #7933, #9645, #11713, #17005, #16643, #20483, #2371, #459, #22287, #3820 ),
 .UNSPECIFIED., .F., .F.,
 ( 4, 2, 2, 2, 2, 2, 2, 4 ),
 ( 0.000000000000000000, 0.0009361184303670160023, 0.001404177645550564986, 0.001872236860734113970, 0.002340296075917663171, 0.002808355291101211938, 0.003276414506284760705, 0.003744473721468309473 ),
 .UNSPECIFIED. ) ;
#2364 = ORIENTED_EDGE ( 'NONE', *, *, #8610, .T. ) ;
#2365 = CARTESIAN_POINT ( 'NONE',  ( -285.2000000000008981, 35.00000000000100897, 107.6499999999999631 ) ) ;
#2366 = CARTESIAN_POINT ( 'NONE',  ( 25.00000000000002132, -52.79999999999942162, 125.0000000000001990 ) ) ;
#2367 = ORIENTED_EDGE ( 'NONE', *, *, #2518, .F. ) ;
#2368 = ORIENTED_EDGE ( 'NONE', *, *, #6862, .T. ) ;
#2369 = FACE_BOUND ( 'NONE', #18057, .T. ) ;
#2370 = CARTESIAN_POINT ( 'NONE',  ( 0.000000000000000000, 0.000000000000000000, 90.00000000000000000 ) ) ;
#2371 = CARTESIAN_POINT ( 'NONE',  ( 282.1290760626065435, 268.3724317483735717, -146.2431816561008873 ) ) ;
#2372 = EDGE_LOOP ( 'NONE', ( #23298, #19118, #826, #16435 ) ) ;
#2373 = EDGE_CURVE ( 'NONE', #12484, #10380, #22971, .T. ) ;
#2374 = CARTESIAN_POINT ( 'NONE',  ( -72.64999999999996305, -87.33333333333338544, 0.000000000000000000 ) ) ;
#2375 = PLANE ( 'NONE',  #17845 ) ;
#2376 = EDGE_CURVE ( 'NONE', #18600, #18149, #23477, .T. ) ;
#2377 = CARTESIAN_POINT ( 'NONE',  ( 93.00000000000000000, 3.000000000000280220, 129.9038105676659711 ) ) ;
#2378 = ADVANCED_FACE ( 'NONE', ( #9097 ), #5469, .F. ) ;
#2379 = ORIENTED_EDGE ( 'NONE', *, *, #9781, .F. ) ;
#2380 = CARTESIAN_POINT ( 'NONE',  ( 280.5908103165959346, 272.0295083325147516, 148.0299054689547233 ) ) ;
#2381 = CARTESIAN_POINT ( 'NONE',  ( 0.000000000000000000, 0.000000000000000000, 150.0000000000000284 ) ) ;
#2382 = EDGE_CURVE ( 'NONE', #1621, #19296, #10822, .T. ) ;
#2383 = UNCERTAINTY_MEASURE_WITH_UNIT (LENGTH_MEASURE( 1.000000000000000082E-05 ), #20647, 'distance_accuracy_value', 'NONE');
#2384 = DIRECTION ( 'NONE',  ( -0.000000000000000000, 1.000000000000000000, 0.000000000000000000 ) ) ;
#2385 = EDGE_LOOP ( 'NONE', ( #14988, #20099 ) ) ;
#2386 = CARTESIAN_POINT ( 'NONE',  ( 0.000000000000000000, 0.000000000000000000, 0.000000000000000000 ) ) ;
#2387 = FACE_OUTER_BOUND ( 'NONE', #12160, .T. ) ;
#2388 = ADVANCED_FACE ( 'NONE', ( #6805 ), #16242, .F. ) ;
#2389 = EDGE_CURVE ( 'NONE', #2213, #16388, #11171, .T. ) ;
#2390 = CARTESIAN_POINT ( 'NONE',  ( -123.1824219776882785, 83.04955713735500922, 32.50000000000641620 ) ) ;
#2391 = PLANE ( 'NONE',  #4733 ) ;
#2392 = ORIENTED_EDGE ( 'NONE', *, *, #171, .F. ) ;
#2393 = EDGE_LOOP ( 'NONE', ( #11641, #12163, #21345, #5733 ) ) ;
#2394 = DIRECTION ( 'NONE',  ( 1.000000000000000000, 0.000000000000000000, 0.000000000000000000 ) ) ;
#2395 = CARTESIAN_POINT ( 'NONE',  ( 0.000000000000000000, 0.000000000000000000, 0.000000000000000000 ) ) ;
#2396 = ORIENTED_EDGE ( 'NONE', *, *, #8047, .F. ) ;
#2397 = LINE ( 'NONE', #6023, #2469 ) ;
#2398 = DIRECTION ( 'NONE',  ( 3.736327486719275871E-16, -1.000000000000000000, 3.469446951953614189E-15 ) ) ;
#2399 = EDGE_LOOP ( 'NONE', ( #14268, #6366, #3728, #21228 ) ) ;
#2400 = CARTESIAN_POINT ( 'NONE',  ( -45.24999999999994316, 100.0000000000000000, 125.0000000000000000 ) ) ;
#2401 = VECTOR ( 'NONE', #13328, 1000.000000000000000 ) ;
#2402 = VERTEX_POINT ( 'NONE', #12876 ) ;
#2403 = DIRECTION ( 'NONE',  ( 0.6964005597823107463, -0.7176533009294141507, 6.982962677686266711E-15 ) ) ;
#2404 = DIRECTION ( 'NONE',  ( 1.000000000000000000, 0.000000000000000000, 0.000000000000000000 ) ) ;
#2405 = VERTEX_POINT ( 'NONE', #19951 ) ;
#2406 = ORIENTED_EDGE ( 'NONE', *, *, #20105, .T. ) ;
#2407 = DIRECTION ( 'NONE',  ( 0.000000000000000000, -0.5000000000000013323, -0.8660254037844380415 ) ) ;
#2408 = CARTESIAN_POINT ( 'NONE',  ( 158.0000000000000284, -500.0000000000000000, 30.00000000000001421 ) ) ;
#2409 = EDGE_CURVE ( 'NONE', #2150, #23349, #8623, .T. ) ;
#2410 = CARTESIAN_POINT ( 'NONE',  ( -15.25457574233255365, -1019.874521950566759, -145.0000000000001137 ) ) ;
#2411 = EDGE_CURVE ( 'NONE', #17092, #2150, #3631, .T. ) ;
#2412 = CARTESIAN_POINT ( 'NONE',  ( 281.3518577254345132, 272.8327955282140920, 145.2494876630256329 ) ) ;
#2413 = DIRECTION ( 'NONE',  ( 1.000000000000000000, 0.000000000000000000, -0.000000000000000000 ) ) ;
#2414 = CYLINDRICAL_SURFACE ( 'NONE', #20904, 4.250000000000000000 ) ;
#2415 = PLANE ( 'NONE',  #11196 ) ;
#2416 = EDGE_LOOP ( 'NONE', ( #12908, #4600, #9788, #20832 ) ) ;
#2417 = CARTESIAN_POINT ( 'NONE',  ( -69.99999999999997158, -112.6666666666667140, 3.000000000000001332 ) ) ;
#2418 = CARTESIAN_POINT ( 'NONE',  ( -0.6169862416623524970, -8.783631307150855605, -7.913704048099795330 ) ) ;
#2419 = VECTOR ( 'NONE', #1210, 1000.000000000000000 ) ;
#2420 =( REPRESENTATION_RELATIONSHIP ('NONE','NONE', #10127, #8847 ) REPRESENTATION_RELATIONSHIP_WITH_TRANSFORMATION ( #473 )SHAPE_REPRESENTATION_RELATIONSHIP( ) );
#2421 = EDGE_LOOP ( 'NONE', ( #2392, #21606, #2207, #2056 ) ) ;
#2422 = CARTESIAN_POINT ( 'NONE',  ( -136.3242110351077372, -1073.761323382753289, -27.75009929603931980 ) ) ;
#2423 = DIRECTION ( 'NONE',  ( 3.469446951953612710E-16, -1.000000000000000000, 0.000000000000000000 ) ) ;
#2424 = EDGE_LOOP ( 'NONE', ( #2273, #11811 ) ) ;
#2425 = CARTESIAN_POINT ( 'NONE',  ( -135.7895026000614109, -1074.740959209980247, 32.50000000000646594 ) ) ;
#2426 = VERTEX_POINT ( 'NONE', #23690 ) ;
#2427 = DIRECTION ( 'NONE',  ( -0.000000000000000000, -0.000000000000000000, 1.000000000000000000 ) ) ;
#2428 = CARTESIAN_POINT ( 'NONE',  ( 282.3059783239181115, 272.4730547946948604, -145.4357574145958552 ) ) ;
#2429 = EDGE_LOOP ( 'NONE', ( #10390, #454, #8131, #8319 ) ) ;
#2430 = AXIS2_PLACEMENT_3D ( 'NONE', #2688, #637, #10084 ) ;
#2431 = CARTESIAN_POINT ( 'NONE',  ( -280.0000000000000568, 269.9999999999999432, 145.0000000000000284 ) ) ;
#2432 = CYLINDRICAL_SURFACE ( 'NONE', #7672, 2.500000000000002220 ) ;
#2433 = CONTEXT_DEPENDENT_SHAPE_REPRESENTATION ( #5707, #4673 ) ;
#2434 = ORIENTED_EDGE ( 'NONE', *, *, #21712, .F. ) ;
#2435 = CIRCLE ( 'NONE', #10954, 2.649999999999971934 ) ;
#2436 = DIRECTION ( 'NONE',  ( -0.000000000000000000, 1.000000000000000000, -3.469446951953613794E-15 ) ) ;
#2437 = EDGE_LOOP ( 'NONE', ( #12043, #17343, #8968, #13517, #4232, #20219, #1875, #17937 ) ) ;
#2438 = CARTESIAN_POINT ( 'NONE',  ( -3.000000000000002665, 0.000000000000000000, 0.000000000000000000 ) ) ;
#2439 = CARTESIAN_POINT ( 'NONE',  ( 1.250000000000000222, 7.938566201357357244, -7.198902722707428481 ) ) ;
#2440 = CARTESIAN_POINT ( 'NONE',  ( 5.000000000000000888, 0.000000000000000000, 0.000000000000000000 ) ) ;
#2441 = DIRECTION ( 'NONE',  ( 1.000000000000000000, 0.000000000000000000, 0.000000000000000000 ) ) ;
#2442 = ORIENTED_EDGE ( 'NONE', *, *, #21402, .T. ) ;
#2443 = CARTESIAN_POINT ( 'NONE',  ( -280.1244295015775378, 273.0299999999999727, -145.6847249064867924 ) ) ;
#2444 =( LENGTH_UNIT ( ) NAMED_UNIT ( * ) SI_UNIT ( .MILLI., .METRE. ) );
#2445 = CONICAL_SURFACE ( 'NONE', #9412, 4.000000000000000000, 0.8911886515913786111 ) ;
#2447 = ORIENTED_EDGE ( 'NONE', *, *, #16828, .T. ) ;
#2446 = EDGE_LOOP ( 'NONE', ( #23698, #9910, #9443, #10299 ) ) ;
#2448 = CARTESIAN_POINT ( 'NONE',  ( -163.0000000000005400, -204.4690652294798383, -29.99999999999344880 ) ) ;
#2449 = CARTESIAN_POINT ( 'NONE',  ( -7.500000000000000000, -4.330127018922198090, -7.422398894150034288 ) ) ;
#2450 = CARTESIAN_POINT ( 'NONE',  ( -44.99999999999997868, -59.79999999999937188, 192.3500000000002217 ) ) ;
#2451 = CARTESIAN_POINT ( 'NONE',  ( 285.2299999999999045, 268.4847249064869743, 146.3684637172358975 ) ) ;
#2452 = DIRECTION ( 'NONE',  ( -3.469446951953614682E-16, 1.000000000000000000, -3.483493295888648978E-15 ) ) ;
#2453 = ORIENTED_EDGE ( 'NONE', *, *, #12890, .F. ) ;
#2454 = LINE ( 'NONE', #4392, #6464 ) ;
#2455 = DIRECTION ( 'NONE',  ( 0.000000000000000000, 0.000000000000000000, -1.000000000000000000 ) ) ;
#2456 =( REPRESENTATION_RELATIONSHIP ('NONE','NONE', #10127, #5587 ) REPRESENTATION_RELATIONSHIP_WITH_TRANSFORMATION ( #5236 )SHAPE_REPRESENTATION_RELATIONSHIP( ) );
#2457 = CARTESIAN_POINT ( 'NONE',  ( 124.3723197571909793, -1092.501637924545321, 32.50000000000647304 ) ) ;
#2458 = ITEM_DEFINED_TRANSFORMATION ( 'NONE', 'NONE', #7304,  #11210 ) ;
#2459 = ORIENTED_EDGE ( 'NONE', *, *, #4998, .T. ) ;
#2461 = CARTESIAN_POINT ( 'NONE',  ( 140.0355749532213281, -37.61698748598472264, 90.00000000000000000 ) ) ;
#2460 = CIRCLE ( 'NONE', #5551, 2.649999999999978595 ) ;
#2462 = EDGE_LOOP ( 'NONE', ( #9554, #19199, #18103 ) ) ;
#2463 = FACE_OUTER_BOUND ( 'NONE', #368, .T. ) ;
#2464 = CIRCLE ( 'NONE', #9037, 2.649999999999985700 ) ;
#2465 = DIRECTION ( 'NONE',  ( -1.000000000000000000, -3.202566417187951028E-16, -6.405132834375902056E-16 ) ) ;
#2466 = ORIENTED_EDGE ( 'NONE', *, *, #13498, .T. ) ;
#2467 = CARTESIAN_POINT ( 'NONE',  ( -19.87455415549606741, 15.25449798579914251, -145.0000000000000000 ) ) ;
#2468 = ORIENTED_EDGE ( 'NONE', *, *, #22574, .F. ) ;
#2469 = VECTOR ( 'NONE', #9783, 1000.000000000000000 ) ;
#2470 = CYLINDRICAL_SURFACE ( 'NONE', #23083, 35.00000000000000711 ) ;
#2471 = CARTESIAN_POINT ( 'NONE',  ( -155.0000000000000284, -204.4690652294799520, -32.49999999999350564 ) ) ;
#2472 = EDGE_CURVE ( 'NONE', #22877, #18582, #8983, .T. ) ;
#2473 = CARTESIAN_POINT ( 'NONE',  ( -312.2000000000014666, -132.2000000000000455, 0.000000000000000000 ) ) ;
#2474 = DIRECTION ( 'NONE',  ( 1.000000000000000000, 0.000000000000000000, 0.000000000000000000 ) ) ;
#2475 = DIRECTION ( 'NONE',  ( 0.000000000000000000, 0.000000000000000000, 1.000000000000000000 ) ) ;
#2476 = EDGE_CURVE ( 'NONE', #22628, #327, #5234, .T. ) ;
#2477 = CARTESIAN_POINT ( 'NONE',  ( 105.0000000000000000, -19.99999999999998934, 3.000000000000001332 ) ) ;
#2478 = ADVANCED_FACE ( 'NONE', ( #12417 ), #3168, .F. ) ;
#2479 = CARTESIAN_POINT ( 'NONE',  ( -7.500000000000000000, 4.730921838224027454, -7.493596905200499592 ) ) ;
#2480 = VERTEX_POINT ( 'NONE', #5349 ) ;
#2481 =( NAMED_UNIT ( * ) PLANE_ANGLE_UNIT ( ) SI_UNIT ( $, .RADIAN. ) );
#2482 = FACE_BOUND ( 'NONE', #3832, .T. ) ;
#2483 = LINE ( 'NONE', #20962, #9282 ) ;
#2484 = ADVANCED_FACE ( 'NONE', ( #1363 ), #18035, .F. ) ;
#2485 = ORIENTED_EDGE ( 'NONE', *, *, #3147, .T. ) ;
#2486 = EDGE_LOOP ( 'NONE', ( #21539, #13879 ) ) ;
#2487 = AXIS2_PLACEMENT_3D ( 'NONE', #16846, #304, #20575 ) ;
#2488 = FACE_OUTER_BOUND ( 'NONE', #11813, .T. ) ;
#2490 = CIRCLE ( 'NONE', #9055, 2.499999999999998668 ) ;
#2489 = CARTESIAN_POINT ( 'NONE',  ( -280.0000000000000568, 272.9999999999999432, -144.9999999999999716 ) ) ;
#2491 = DIRECTION ( 'NONE',  ( 1.000000000000000000, 0.000000000000000000, -0.000000000000000000 ) ) ;
#2492 = VECTOR ( 'NONE', #13882, 1000.000000000000000 ) ;
#2493 = ORIENTED_EDGE ( 'NONE', *, *, #16579, .T. ) ;
#2494 = CARTESIAN_POINT ( 'NONE',  ( -2.682243648011671588, -3.070208061305317759, -0.04852650426602272971 ) ) ;
#2495 = DIRECTION ( 'NONE',  ( 1.000000000000000000, 0.000000000000000000, 0.000000000000000000 ) ) ;
#2496 = DIRECTION ( 'NONE',  ( -1.000000000000000000, -0.000000000000000000, -0.000000000000000000 ) ) ;
#2497 = VERTEX_POINT ( 'NONE', #8874 ) ;
#2498 = LINE ( 'NONE', #4057, #10658 ) ;
#2499 = DIRECTION ( 'NONE',  ( 0.000000000000000000, 0.000000000000000000, 1.000000000000000000 ) ) ;
#2500 = SURFACE_STYLE_USAGE ( .BOTH. , #21334 ) ;
#2501 = VERTEX_POINT ( 'NONE', #20080 ) ;
#2502 = CIRCLE ( 'NONE', #960, 2.500000000000000444 ) ;
#2503 = DIRECTION ( 'NONE',  ( -1.000000000000000000, 3.495664435217746987E-15, 0.000000000000000000 ) ) ;
#2504 = DIRECTION ( 'NONE',  ( -1.350636282998972974E-14, 0.000000000000000000, -1.000000000000000000 ) ) ;
#2505 = FACE_OUTER_BOUND ( 'NONE', #10784, .T. ) ;
#2506 = CIRCLE ( 'NONE', #1718, 2.649999999999971934 ) ;
#2507 = UNCERTAINTY_MEASURE_WITH_UNIT (LENGTH_MEASURE( 1.000000000000000082E-05 ), #10014, 'distance_accuracy_value', 'NONE');
#2508 = ADVANCED_FACE ( 'NONE', ( #14428 ), #3525, .F. ) ;
#2509 = ORIENTED_EDGE ( 'NONE', *, *, #11719, .T. ) ;
#2510 = ORIENTED_EDGE ( 'NONE', *, *, #2373, .T. ) ;
#2511 = CARTESIAN_POINT ( 'NONE',  ( -122.8605704798722087, 82.74225173005940803, -32.05499999999356930 ) ) ;
#2512 = FACE_OUTER_BOUND ( 'NONE', #9395, .T. ) ;
#2513 = EDGE_CURVE ( 'NONE', #8431, #7697, #1709, .T. ) ;
#2514 = ADVANCED_FACE ( 'NONE', ( #14665, #5002 ), #19716, .T. ) ;
#2515 = AXIS2_PLACEMENT_3D ( 'NONE', #3941, #7574, #9521 ) ;
#2516 = ORIENTED_EDGE ( 'NONE', *, *, #558, .T. ) ;
#2517 = DIRECTION ( 'NONE',  ( 0.000000000000000000, 0.000000000000000000, -1.000000000000000000 ) ) ;
#2518 = EDGE_CURVE ( 'NONE', #12660, #5442, #23460, .T. ) ;
#2519 = PLANE ( 'NONE',  #19938 ) ;
#2520 = PRODUCT_RELATED_PRODUCT_CATEGORY ( 'part', '', ( #20194 ) ) ;
#2521 = EDGE_LOOP ( 'NONE', ( #15122, #7804, #420, #6250 ) ) ;
#2522 = DIRECTION ( 'NONE',  ( 0.000000000000000000, 0.000000000000000000, 1.000000000000000000 ) ) ;
#2523 = VECTOR ( 'NONE', #1194, 1000.000000000000114 ) ;
#2524 = ORIENTED_EDGE ( 'NONE', *, *, #15478, .T. ) ;
#2525 = CARTESIAN_POINT ( 'NONE',  ( 100.0000000000000000, 270.0000000000000000, -144.9999999999999716 ) ) ;
#2526 = PLANE ( 'NONE',  #3593 ) ;
#2527 = ORIENTED_EDGE ( 'NONE', *, *, #15560, .F. ) ;
#2528 = EDGE_LOOP ( 'NONE', ( #23738, #21267 ) ) ;
#2529 = LINE ( 'NONE', #6033, #13147 ) ;
#2530 = PRODUCT_DEFINITION_SHAPE ( 'NONE', 'NONE',  #23853 ) ;
#2531 = LINE ( 'NONE', #18818, #20422 ) ;
#2532 = AXIS2_PLACEMENT_3D ( 'NONE', #17832, #23249, #10011 ) ;
#2533 = PLANE ( 'NONE',  #8822 ) ;
#2534 = DIRECTION ( 'NONE',  ( -0.000000000000000000, 1.000000000000000000, -3.469446951953613794E-15 ) ) ;
#2535 = VECTOR ( 'NONE', #1684, 1000.000000000000000 ) ;
#2536 = CARTESIAN_POINT ( 'NONE',  ( 2.500000000000000000, 1.178949249685218081, 2.041999999999998483 ) ) ;
#2537 = VERTEX_POINT ( 'NONE', #9226 ) ;
#2538 = CARTESIAN_POINT ( 'NONE',  ( -34.75000000000005684, 100.0000000000000000, -145.0000000000000284 ) ) ;
#2539 =( LENGTH_UNIT ( ) NAMED_UNIT ( * ) SI_UNIT ( .MILLI., .METRE. ) );
#2540 = AXIS2_PLACEMENT_3D ( 'NONE', #3175, #6811, #5010 ) ;
#2541 = B_SPLINE_CURVE_WITH_KNOTS ( 'NONE', 3,
 ( #14118, #3096, #15798, #15568, #1033 ),
 .UNSPECIFIED., .F., .F.,
 ( 4, 1, 4 ),
 ( 0.000000000000000000, 0.002309401076758505356, 0.004618802153517010713 ),
 .UNSPECIFIED. ) ;
#2542 = ORIENTED_EDGE ( 'NONE', *, *, #13946, .F. ) ;
#2543 = FACE_BOUND ( 'NONE', #378, .T. ) ;
#2544 = VERTEX_POINT ( 'NONE', #20541 ) ;
#2545 = DIRECTION ( 'NONE',  ( -0.000000000000000000, 0.000000000000000000, 1.000000000000000000 ) ) ;
#2546 = ADVANCED_FACE ( 'NONE', ( #18847 ), #11188, .F. ) ;
#2547 = EDGE_CURVE ( 'NONE', #19084, #13384, #18503, .T. ) ;
#2548 = VERTEX_POINT ( 'NONE', #5583 ) ;
#2549 = VECTOR ( 'NONE', #11554, 1000.000000000000000 ) ;
#2551 = EDGE_CURVE ( 'NONE', #3909, #16080, #4116, .T. ) ;
#2550 = LINE ( 'NONE', #13707, #11792 ) ;
#2552 = CARTESIAN_POINT ( 'NONE',  ( 283.5570580646225949, 271.5968359015655551, -145.7154581756739162 ) ) ;
#2553 = ORIENTED_EDGE ( 'NONE', *, *, #3097, .F. ) ;
#2554 = CARTESIAN_POINT ( 'NONE',  ( -280.4976310729379065, 272.3699028110927429, 147.6339272673398284 ) ) ;
#2555 = DIRECTION ( 'NONE',  ( 1.211350928885223478E-30, -3.491481338843133355E-15, -1.000000000000000000 ) ) ;
#2556 = EDGE_LOOP ( 'NONE', ( #1169, #20317, #11260, #17051 ) ) ;
#2557 = LINE ( 'NONE', #15384, #17979 ) ;
#2558 = CARTESIAN_POINT ( 'NONE',  ( -281.4928932188135491, 267.7999999999999545, 147.1999999999999886 ) ) ;
#2559 = LINE ( 'NONE', #4620, #1080 ) ;
#2560 = CARTESIAN_POINT ( 'NONE',  ( 0.2500000000000002220, 5.204748896376238866E-16, -4.249999999999979572 ) ) ;
#2561 = ORIENTED_EDGE ( 'NONE', *, *, #9886, .T. ) ;
#2562 = DIRECTION ( 'NONE',  ( -1.000000000000000000, -0.000000000000000000, -0.000000000000000000 ) ) ;
#2563 = AXIS2_PLACEMENT_3D ( 'NONE', #20779, #22586, #11657 ) ;
#2565 = ORIENTED_EDGE ( 'NONE', *, *, #1074, .F. ) ;
#2564 = ORIENTED_EDGE ( 'NONE', *, *, #22136, .F. ) ;
#2566 = DIRECTION ( 'NONE',  ( -1.000000000000000000, 1.408839003528726857E-14, 0.000000000000000000 ) ) ;
#2567 = CARTESIAN_POINT ( 'NONE',  ( -146.4450000000005332, -784.4690652294799520, -32.49999999999356248 ) ) ;
#2568 = CARTESIAN_POINT ( 'NONE',  ( 132.0389103176324568, 81.18340533128207426, -31.99040335529153367 ) ) ;
#2569 = CARTESIAN_POINT ( 'NONE',  ( 285.0646579186752660, 269.1610889986682196, 146.2440776823445958 ) ) ;
#2570 = CARTESIAN_POINT ( 'NONE',  ( -282.2000000000000455, 267.7999999999999545, -146.4928932188134354 ) ) ;
#2571 = EDGE_CURVE ( 'NONE', #12463, #19820, #7626, .T. ) ;
#2572 = ORIENTED_EDGE ( 'NONE', *, *, #6969, .T. ) ;
#2573 = AXIS2_PLACEMENT_3D ( 'NONE', #18121, #3715, #20260 ) ;
#2574 = DIRECTION ( 'NONE',  ( 0.000000000000000000, 0.000000000000000000, 1.000000000000000000 ) ) ;
#2575 = EDGE_CURVE ( 'NONE', #3378, #2646, #3889, .T. ) ;
#2576 = VECTOR ( 'NONE', #19776, 1000.000000000000000 ) ;
#2577 = FACE_OUTER_BOUND ( 'NONE', #18376, .T. ) ;
#2578 = DIRECTION ( 'NONE',  ( -1.000000000000000000, 0.000000000000000000, 0.000000000000000000 ) ) ;
#2579 = ORIENTED_EDGE ( 'NONE', *, *, #13734, .F. ) ;
#2580 = FACE_OUTER_BOUND ( 'NONE', #2393, .T. ) ;
#2581 = ORIENTED_EDGE ( 'NONE', *, *, #18641, .T. ) ;
#2582 = FACE_OUTER_BOUND ( 'NONE', #245, .T. ) ;
#2583 = CARTESIAN_POINT ( 'NONE',  ( -105.0000000000000142, 30.00000000000001421, 3.000000000000000000 ) ) ;
#2584 = EDGE_LOOP ( 'NONE', ( #14668, #14902, #12639, #2722, #11589 ) ) ;
#2585 = DIRECTION ( 'NONE',  ( -0.000000000000000000, 0.4999999999999979461, -0.8660254037844397068 ) ) ;
#2586 = ORIENTED_EDGE ( 'NONE', *, *, #22003, .F. ) ;
#2587 = CARTESIAN_POINT ( 'NONE',  ( -100.0000000000000000, -1420.000000000000000, -145.0000000000001705 ) ) ;
#2588 = FACE_OUTER_BOUND ( 'NONE', #5104, .T. ) ;
#2589 = DIRECTION ( 'NONE',  ( 6.640089860198304064E-16, 1.000000000000000000, -4.183096374613631247E-18 ) ) ;
#2590 = DIRECTION ( 'NONE',  ( 0.5000000000000022204, 0.8660254037844374864, -0.000000000000000000 ) ) ;
#2591 = FACE_OUTER_BOUND ( 'NONE', #2128, .T. ) ;
#2592 = CARTESIAN_POINT ( 'NONE',  ( -1.391697335622809950, -4.043246145443391448, -3.503898532754372575 ) ) ;
#2593 = AXIS2_PLACEMENT_3D ( 'NONE', #14134, #8673, #5060 ) ;
#2594 = LINE ( 'NONE', #11945, #16704 ) ;
#2595 = ORIENTED_EDGE ( 'NONE', *, *, #1246, .T. ) ;
#2596 = SURFACE_STYLE_USAGE ( .BOTH. , #10225 ) ;
#2597 = CARTESIAN_POINT ( 'NONE',  ( 60.00000000000000000, -59.80000000000001137, 2.159765843450962666E-13 ) ) ;
#2598 = CARTESIAN_POINT ( 'NONE',  ( -4.197477534772231955, 0.8522413273724368521, -3.505042416683225692 ) ) ;
#2599 = VECTOR ( 'NONE', #1773, 1000.000000000000114 ) ;
#2600 = ORIENTED_EDGE ( 'NONE', *, *, #4041, .F. ) ;
#2601 = EDGE_CURVE ( 'NONE', #1295, #18149, #20390, .T. ) ;
#2602 = ORIENTED_EDGE ( 'NONE', *, *, #17978, .T. ) ;
#2603 = AXIS2_PLACEMENT_3D ( 'NONE', #15932, #23273, #4930 ) ;
#2604 = DIRECTION ( 'NONE',  ( -0.000000000000000000, -0.000000000000000000, 1.000000000000000000 ) ) ;
#2605 = LINE ( 'NONE', #4311, #15382 ) ;
#2606 = DIRECTION ( 'NONE',  ( 1.000000000000000000, 0.000000000000000000, -0.000000000000000000 ) ) ;
#2607 = CARTESIAN_POINT ( 'NONE',  ( 131.5158088764650586, 82.02799531629221974, 30.16873261443286580 ) ) ;
#2608 = PLANE ( 'NONE',  #19356 ) ;
#2609 = ADVANCED_FACE ( 'NONE', ( #11298 ), #16589, .F. ) ;
#2610 = AXIS2_PLACEMENT_3D ( 'NONE', #21430, #4667, #15778 ) ;
#2611 = CARTESIAN_POINT ( 'NONE',  ( -3.750000000000007105, -6.495190528383289141, 0.000000000000000000 ) ) ;
#2612 = EDGE_LOOP ( 'NONE', ( #8421, #21186, #22709, #21255 ) ) ;
#2613 = DIRECTION ( 'NONE',  ( 0.000000000000000000, 0.000000000000000000, -1.000000000000000000 ) ) ;
#2614 = DIRECTION ( 'NONE',  ( -4.625929269271485914E-16, -3.469446951953614583E-15, -1.000000000000000000 ) ) ;
#2615 = EDGE_CURVE ( 'NONE', #9524, #14070, #7508, .T. ) ;
#2616 = DIRECTION ( 'NONE',  ( 1.000000000000000000, 0.000000000000000000, 0.000000000000000000 ) ) ;
#2617 = AXIS2_PLACEMENT_3D ( 'NONE', #196, #7549, #20468 ) ;
#2618 = ORIENTED_EDGE ( 'NONE', *, *, #20520, .F. ) ;
#2619 = CARTESIAN_POINT ( 'NONE',  ( 281.8958543268121844, 268.8927021017106540, -145.9952621458755857 ) ) ;
#2620 = VECTOR ( 'NONE', #3115, 1000.000000000000114 ) ;
#2621 = ITEM_DEFINED_TRANSFORMATION ( 'NONE', 'NONE', #19266,  #11210 ) ;
#2622 = CARTESIAN_POINT ( 'NONE',  ( -155.0000000000000284, -784.4690652294798383, -32.49999999999350564 ) ) ;
#2623 = CARTESIAN_POINT ( 'NONE',  ( -146.4450000000005332, -494.4690652294800657, -29.99999999999356248 ) ) ;
#2624 = FACE_OUTER_BOUND ( 'NONE', #20466, .T. ) ;
#2625 = ORIENTED_EDGE ( 'NONE', *, *, #10506, .F. ) ;
#2626 = ORIENTED_EDGE ( 'NONE', *, *, #3852, .T. ) ;
#2627 = DIRECTION ( 'NONE',  ( 0.000000000000000000, 0.000000000000000000, 1.000000000000000000 ) ) ;
#2628 = DIRECTION ( 'NONE',  ( -0.9423651898111408132, -0.3345860861306287348, 6.982962677686266711E-15 ) ) ;
#2629 = EDGE_LOOP ( 'NONE', ( #2051, #6281 ) ) ;
#2630 = VECTOR ( 'NONE', #15357, 1000.000000000000000 ) ;
#2631 = VECTOR ( 'NONE', #3825, 1000.000000000000000 ) ;
#2632 = AXIS2_PLACEMENT_3D ( 'NONE', #12238, #7885, #20671 ) ;
#2633 = ORIENTED_EDGE ( 'NONE', *, *, #5098, .T. ) ;
#2634 = CARTESIAN_POINT ( 'NONE',  ( 7.500000000000000000, 4.330127018922199866, -1.000000000000000888 ) ) ;
#2635 = VECTOR ( 'NONE', #21326, 1000.000000000000000 ) ;
#2636 = EDGE_CURVE ( 'NONE', #21483, #4937, #16940, .T. ) ;
#2637 = CARTESIAN_POINT ( 'NONE',  ( -24.99999999999998579, -37.41657386773942306, 169.9999999999999716 ) ) ;
#2638 = ORIENTED_EDGE ( 'NONE', *, *, #16272, .T. ) ;
#2639 = EDGE_CURVE ( 'NONE', #18956, #2402, #3052, .T. ) ;
#2640 = PLANE ( 'NONE',  #17162 ) ;
#2641 = ORIENTED_EDGE ( 'NONE', *, *, #12655, .F. ) ;
#2642 = FACE_OUTER_BOUND ( 'NONE', #20715, .T. ) ;
#2643 = EDGE_CURVE ( 'NONE', #20268, #22534, #20021, .T. ) ;
#2644 = LINE ( 'NONE', #6511, #4380 ) ;
#2645 = ORIENTED_EDGE ( 'NONE', *, *, #6630, .T. ) ;
#2646 = VERTEX_POINT ( 'NONE', #16812 ) ;
#2647 = DIRECTION ( 'NONE',  ( 0.9289202219288174023, 0.3702799228849934510, 6.982962677686266711E-15 ) ) ;
#2648 = EDGE_CURVE ( 'NONE', #7824, #6807, #268, .T. ) ;
#2649 = MECHANICAL_DESIGN_GEOMETRIC_PRESENTATION_REPRESENTATION (  '', ( #17334 ), #12363 ) ;
#2650 = CARTESIAN_POINT ( 'NONE',  ( -281.4301685938042965, 268.1431883596741841, -150.1999999999999318 ) ) ;
#2652 = CIRCLE ( 'NONE', #21166, 2.500000000000002220 ) ;
#2651 = MECHANICAL_DESIGN_GEOMETRIC_PRESENTATION_REPRESENTATION (  '', ( #5739 ), #8063 ) ;
#2653 = AXIS2_PLACEMENT_3D ( 'NONE', #18912, #22648, #19018 ) ;
#2654 = VECTOR ( 'NONE', #23339, 1000.000000000000000 ) ;
#2655 = AXIS2_PLACEMENT_3D ( 'NONE', #586, #11852, #13669 ) ;
#2656 = FACE_OUTER_BOUND ( 'NONE', #3132, .T. ) ;
#2657 = VECTOR ( 'NONE', #10679, 1000.000000000000000 ) ;
#2658 = EDGE_CURVE ( 'NONE', #2501, #12643, #22364, .T. ) ;
#2659 = PLANE ( 'NONE',  #4593 ) ;
#2660 = ORIENTED_EDGE ( 'NONE', *, *, #13454, .F. ) ;
#2661 = CARTESIAN_POINT ( 'NONE',  ( -3.080866544137490504, -6.881514909249304424, -7.026396753507435200 ) ) ;
#2662 =( NAMED_UNIT ( * ) PLANE_ANGLE_UNIT ( ) SI_UNIT ( $, .RADIAN. ) );
#2663 = ADVANCED_FACE ( 'NONE', ( #5831 ), #2317, .T. ) ;
#2664 = AXIS2_PLACEMENT_3D ( 'NONE', #12447, #16140, #4785 ) ;
#2665 = UNCERTAINTY_MEASURE_WITH_UNIT (LENGTH_MEASURE( 1.000000000000000082E-05 ), #1814, 'distance_accuracy_value', 'NONE');
#2666 = ORIENTED_EDGE ( 'NONE', *, *, #16101, .F. ) ;
#2667 = CARTESIAN_POINT ( 'NONE',  ( -37.61698748598514896, -140.0355749532212428, -2.775557561562891351E-14 ) ) ;
#2668 = AXIS2_PLACEMENT_3D ( 'NONE', #19213, #21283, #10439 ) ;
#2669 = CARTESIAN_POINT ( 'NONE',  ( 11.08409875733031136, -22.46856765614143825, -145.0000000000000000 ) ) ;
#2670 = AXIS2_PLACEMENT_3D ( 'NONE', #17531, #19703, #21287 ) ;
#2671 = ORIENTED_EDGE ( 'NONE', *, *, #11106, .T. ) ;
#2672 = AXIS2_PLACEMENT_3D ( 'NONE', #9268, #7797, #16629 ) ;
#2673 = CARTESIAN_POINT ( 'NONE',  ( -67.34999999999996589, -112.6666666666667140, 3.000000000000000000 ) ) ;
#2674 = CIRCLE ( 'NONE', #13520, 2.649999999999999467 ) ;
#2675 = AXIS2_PLACEMENT_3D ( 'NONE', #1240, #6317, #19231 ) ;
#2676 = CARTESIAN_POINT ( 'NONE',  ( -51.87806360044817922, 135.4018704341556258, -2.775557561562891351E-14 ) ) ;
#2677 = CIRCLE ( 'NONE', #11966, 2.649999999999978595 ) ;
#2678 = VECTOR ( 'NONE', #22928, 1000.000000000000000 ) ;
#2679 = ORIENTED_EDGE ( 'NONE', *, *, #6053, .T. ) ;
#2680 = EDGE_CURVE ( 'NONE', #18466, #16256, #14646, .T. ) ;
#2681 = DIRECTION ( 'NONE',  ( 0.7071067811865416886, 0.000000000000000000, -0.7071067811865532349 ) ) ;
#2682 = CARTESIAN_POINT ( 'NONE',  ( 235.0000000000000284, -557.0000000000000000, 56.99999999999998579 ) ) ;
#2683 = EDGE_CURVE ( 'NONE', #15535, #5442, #9705, .T. ) ;
#2684 = ORIENTED_EDGE ( 'NONE', *, *, #6466, .F. ) ;
#2685 = UNCERTAINTY_MEASURE_WITH_UNIT (LENGTH_MEASURE( 1.000000000000000082E-05 ), #414, 'distance_accuracy_value', 'NONE');
#2686 = CARTESIAN_POINT ( 'NONE',  ( 1.500000000000000000, 11.99999999999999822, 200.0000000000000000 ) ) ;
#2687 = ADVANCED_FACE ( 'NONE', ( #15260 ), #22593, .F. ) ;
#2688 = CARTESIAN_POINT ( 'NONE',  ( 70.00000000000000000, -87.33333333333332860, 148.0000000000000000 ) ) ;
#2689 = CARTESIAN_POINT ( 'NONE',  ( -282.2000000000012960, -74.99999999999899103, -90.00000000000000000 ) ) ;
#2690 = EDGE_CURVE ( 'NONE', #14056, #3521, #4725, .T. ) ;
#2691 = DIRECTION ( 'NONE',  ( -1.000000000000000000, -0.000000000000000000, -0.000000000000000000 ) ) ;
#2692 = VERTEX_POINT ( 'NONE', #20912 ) ;
#2694 = AXIS2_PLACEMENT_3D ( 'NONE', #9686, #4584, #15123 ) ;
#2693 = AXIS2_PLACEMENT_3D ( 'NONE', #3541, #11198, #9117 ) ;
#2695 = CARTESIAN_POINT ( 'NONE',  ( 2.500000000000000000, -2.357898499370432166, 3.035766082959412415E-15 ) ) ;
#2696 = EDGE_CURVE ( 'NONE', #4477, #16291, #13560, .T. ) ;
#2697 = AXIS2_PLACEMENT_3D ( 'NONE', #9721, #15396, #17076 ) ;
#2698 = AXIS2_PLACEMENT_3D ( 'NONE', #12141, #12505, #19814 ) ;
#2699 = CIRCLE ( 'NONE', #20036, 2.499999999999946709 ) ;
#2701 = ORIENTED_EDGE ( 'NONE', *, *, #22909, .F. ) ;
#2700 = ORIENTED_EDGE ( 'NONE', *, *, #15773, .T. ) ;
#2702 = DIRECTION ( 'NONE',  ( 6.486615240276975916E-15, 2.585650881802458380E-15, -1.000000000000000000 ) ) ;
#2703 = CARTESIAN_POINT ( 'NONE',  ( -0.6250000000000001110, 8.299410119600874935, -7.298562697733108173 ) ) ;
#2704 = FACE_OUTER_BOUND ( 'NONE', #19121, .T. ) ;
#2705 = DIRECTION ( 'NONE',  ( 0.000000000000000000, 0.000000000000000000, 1.000000000000000000 ) ) ;
#2706 = CARTESIAN_POINT ( 'NONE',  ( -285.2000000000000455, 268.4807971656550194, -146.3684637452624884 ) ) ;
#2707 = ORIENTED_EDGE ( 'NONE', *, *, #6136, .F. ) ;
#2708 = DIRECTION ( 'NONE',  ( 0.000000000000000000, 0.000000000000000000, -1.000000000000000000 ) ) ;
#2709 = PRODUCT_DEFINITION_FORMATION_WITH_SPECIFIED_SOURCE ( 'ANY', '', #2824, .NOT_KNOWN. ) ;
#2710 = DIRECTION ( 'NONE',  ( 0.3090169943749441761, 0.9510565162951546414, 0.000000000000000000 ) ) ;
#2711 = DIRECTION ( 'NONE',  ( 0.000000000000000000, 0.000000000000000000, 1.000000000000000000 ) ) ;
#2712 = AXIS2_PLACEMENT_3D ( 'NONE', #11711, #20855, #4176 ) ;
#2713 = ORIENTED_EDGE ( 'NONE', *, *, #21503, .T. ) ;
#2714 = CIRCLE ( 'NONE', #18909, 2.500000000000000444 ) ;
#2715 = AXIS2_PLACEMENT_3D ( 'NONE', #22993, #6348, #10119 ) ;
#2716 = LINE ( 'NONE', #21061, #895 ) ;
#2717 = ORIENTED_EDGE ( 'NONE', *, *, #22537, .T. ) ;
#2718 = CARTESIAN_POINT ( 'NONE',  ( 0.000000000000000000, 0.000000000000000000, 124.9999999999999716 ) ) ;
#2719 = DIRECTION ( 'NONE',  ( 0.000000000000000000, -1.000000000000000000, 0.000000000000000000 ) ) ;
#2720 = ORIENTED_EDGE ( 'NONE', *, *, #16990, .F. ) ;
#2721 = CARTESIAN_POINT ( 'NONE',  ( 6.902527771671632451, 4.675077770780898589, -0.7026937717022819774 ) ) ;
#2722 = ORIENTED_EDGE ( 'NONE', *, *, #14313, .T. ) ;
#2723 = DIRECTION ( 'NONE',  ( 0.000000000000000000, 0.000000000000000000, -1.000000000000000000 ) ) ;
#2724 = CARTESIAN_POINT ( 'NONE',  ( 0.000000000000000000, 5.051668046482832750E-16, -4.000000000000000000 ) ) ;
#2725 = EDGE_CURVE ( 'NONE', #15958, #4200, #11618, .T. ) ;
#2726 = CARTESIAN_POINT ( 'NONE',  ( 281.9771650631952866, 268.7755899421579784, 146.0571594757292928 ) ) ;
#2727 = ADVANCED_FACE ( 'NONE', ( #13956 ), #18089, .F. ) ;
#2728 = DIRECTION ( 'NONE',  ( 1.000000000000000000, 0.000000000000000000, 0.000000000000000000 ) ) ;
#2729 = CARTESIAN_POINT ( 'NONE',  ( 0.000000000000000000, 0.000000000000000000, 0.000000000000000000 ) ) ;
#2730 = EDGE_CURVE ( 'NONE', #5940, #15926, #4241, .T. ) ;
#2731 = ORIENTED_EDGE ( 'NONE', *, *, #843, .F. ) ;
#2732 = CARTESIAN_POINT ( 'NONE',  ( -136.9911991620662661, -1072.514904345033301, 29.67072815018525844 ) ) ;
#2733 = LINE ( 'NONE', #4774, #13446 ) ;
#2734 = CARTESIAN_POINT ( 'NONE',  ( -4.000000000000000000, -1.680117682357936904, -3.316611593218794951 ) ) ;
#2735 = EDGE_LOOP ( 'NONE', ( #4395, #3923 ) ) ;
#2736 = VERTEX_POINT ( 'NONE', #8483 ) ;
#2737 = CARTESIAN_POINT ( 'NONE',  ( 5.200000000000002842, 0.000000000000000000, 0.000000000000000000 ) ) ;
#2738 = CARTESIAN_POINT ( 'NONE',  ( 146.4449999999997942, -801.0618695410399823, 30.00000000000641975 ) ) ;
#2740 = DIRECTION ( 'NONE',  ( -1.000000000000000000, 1.408839003528726857E-14, 6.982962677686266711E-15 ) ) ;
#2739 = PRODUCT_DEFINITION_SHAPE ( 'NONE', 'NONE',  #23824 ) ;
#2741 = CARTESIAN_POINT ( 'NONE',  ( 132.4977819882881249, 80.43276747726562803, 27.56549073392523042 ) ) ;
#2742 = CARTESIAN_POINT ( 'NONE',  ( 5.000000000000000000, 4.685197434473814759, -5.637851296924623057E-15 ) ) ;
#2743 = DIRECTION ( 'NONE',  ( 0.000000000000000000, 0.000000000000000000, -1.000000000000000000 ) ) ;
#2744 = VERTEX_POINT ( 'NONE', #23196 ) ;
#2745 = DIRECTION ( 'NONE',  ( 1.000000000000000000, 0.000000000000000000, 0.000000000000000000 ) ) ;
#2746 = CARTESIAN_POINT ( 'NONE',  ( -100.0000000000000000, -1420.000000000000000, 144.9999999999998295 ) ) ;
#2747 = DIRECTION ( 'NONE',  ( -0.000000000000000000, 0.000000000000000000, 1.000000000000000000 ) ) ;
#2748 = ORIENTED_EDGE ( 'NONE', *, *, #13603, .T. ) ;
#2749 = LINE ( 'NONE', #10135, #18878 ) ;
#2750 = APPLICATION_CONTEXT ( 'automotive_design' ) ;
#2751 = DIRECTION ( 'NONE',  ( 0.000000000000000000, 0.000000000000000000, -1.000000000000000000 ) ) ;
#2752 = CARTESIAN_POINT ( 'NONE',  ( -5.000000000000000888, 6.123233995736767268E-16, -10.00000000000000000 ) ) ;
#2753 = CARTESIAN_POINT ( 'NONE',  ( -282.3059783239183389, 272.4730547946946899, 145.4357574145959120 ) ) ;
#2754 = EDGE_CURVE ( 'NONE', #18250, #14819, #6659, .T. ) ;
#2755 = ORIENTED_EDGE ( 'NONE', *, *, #2275, .T. ) ;
#2756 = VERTEX_POINT ( 'NONE', #7997 ) ;
#2757 = DIRECTION ( 'NONE',  ( 3.469446951953614682E-16, -1.000000000000000000, 3.483493295888648978E-15 ) ) ;
#2758 = CARTESIAN_POINT ( 'NONE',  ( -3.823040241140506157E-16, -8.660254037844397956, -7.564338275809345369 ) ) ;
#2759 = ORIENTED_EDGE ( 'NONE', *, *, #7009, .T. ) ;
#2760 = EDGE_LOOP ( 'NONE', ( #18334, #15913 ) ) ;
#2761 = CARTESIAN_POINT ( 'NONE',  ( -31.74999999999994316, 0.000000000000000000, 0.000000000000000000 ) ) ;
#2762 = DIRECTION ( 'NONE',  ( -0.000000000000000000, 1.000000000000000000, -3.469446951953613794E-15 ) ) ;
#2763 = ORIENTED_EDGE ( 'NONE', *, *, #22787, .F. ) ;
#2764 = DIRECTION ( 'NONE',  ( 1.000000000000000000, 0.000000000000000000, 0.000000000000000000 ) ) ;
#2765 = VERTEX_POINT ( 'NONE', #15377 ) ;
#2766 = DIRECTION ( 'NONE',  ( -0.000000000000000000, 1.000000000000000000, -3.469446951953613794E-15 ) ) ;
#2767 = FACE_BOUND ( 'NONE', #7448, .T. ) ;
#2768 = EDGE_LOOP ( 'NONE', ( #20010, #7873, #12545, #10162, #19871 ) ) ;
#2769 = ORIENTED_EDGE ( 'NONE', *, *, #12380, .F. ) ;
#2770 = CARTESIAN_POINT ( 'NONE',  ( 0.5449313310647804220, 4.304185902836899835, -3.316620875263383894 ) ) ;
#2771 = CARTESIAN_POINT ( 'NONE',  ( 93.00000000000000000, -149.9999999999996874, 3.000000000000002665 ) ) ;
#2772 = FACE_OUTER_BOUND ( 'NONE', #2800, .T. ) ;
#2773 = ADVANCED_FACE ( 'NONE', ( #22721 ), #6190, .F. ) ;
#2774 = ORIENTED_EDGE ( 'NONE', *, *, #15773, .F. ) ;
#2775 = CARTESIAN_POINT ( 'NONE',  ( -6.484173630544109557, -4.916614646775610886, -7.642786413610934915 ) ) ;
#2776 = SURFACE_STYLE_FILL_AREA ( #19684 ) ;
#2777 = EDGE_CURVE ( 'NONE', #9321, #21395, #16651, .T. ) ;
#2778 = EDGE_CURVE ( 'NONE', #4532, #8574, #10433, .T. ) ;
#2779 = VERTEX_POINT ( 'NONE', #18322 ) ;
#2780 = EDGE_CURVE ( 'NONE', #8322, #19974, #4844, .T. ) ;
#2781 = VECTOR ( 'NONE', #686, 1000.000000000000000 ) ;
#2782 = ORIENTED_EDGE ( 'NONE', *, *, #15460, .F. ) ;
#2783 = CARTESIAN_POINT ( 'NONE',  ( 23.72528575883189816, -8.050112875864174455, -145.0000000000000000 ) ) ;
#2784 = ORIENTED_EDGE ( 'NONE', *, *, #5582, .F. ) ;
#2785 = CARTESIAN_POINT ( 'NONE',  ( 0.000000000000000000, 0.000000000000000000, 0.000000000000000000 ) ) ;
#2786 = PLANE ( 'NONE',  #17177 ) ;
#2787 = ORIENTED_EDGE ( 'NONE', *, *, #8816, .F. ) ;
#2788 = CARTESIAN_POINT ( 'NONE',  ( -280.8708543776413080, 269.1520027839447948, 146.7592670532760053 ) ) ;
#2789 =( NAMED_UNIT ( * ) SI_UNIT ( $, .STERADIAN. ) SOLID_ANGLE_UNIT ( ) );
#2790 = ORIENTED_EDGE ( 'NONE', *, *, #2409, .T. ) ;
#2791 = CARTESIAN_POINT ( 'NONE',  ( -285.2000000000007276, 75.00000000000100897, -90.00000000000000000 ) ) ;
#2792 = DIRECTION ( 'NONE',  ( 0.000000000000000000, 1.000000000000000000, 0.000000000000000000 ) ) ;
#2793 = DIRECTION ( 'NONE',  ( 1.000000000000000000, 0.000000000000000000, 0.000000000000000000 ) ) ;
#2794 = AXIS2_PLACEMENT_3D ( 'NONE', #15332, #2259, #4328 ) ;
#2795 = DIRECTION ( 'NONE',  ( -0.000000000000000000, -0.000000000000000000, 1.000000000000000000 ) ) ;
#2796 = ORIENTED_EDGE ( 'NONE', *, *, #6247, .F. ) ;
#2797 = CARTESIAN_POINT ( 'NONE',  ( 5.000000000000004441, 5.204748896376250699E-16, -4.250000000000000000 ) ) ;
#2798 = CONTEXT_DEPENDENT_SHAPE_REPRESENTATION ( #6768, #14350 ) ;
#2800 = EDGE_LOOP ( 'NONE', ( #3455, #7439, #7275, #18732 ) ) ;
#2799 = ORIENTED_EDGE ( 'NONE', *, *, #863, .T. ) ;
#2801 = DIRECTION ( 'NONE',  ( 6.982962677686266711E-15, 0.000000000000000000, -1.000000000000000000 ) ) ;
#2802 = CARTESIAN_POINT ( 'NONE',  ( 7.499999999998625100, 3.882635837268474166, -7.781684861371460649 ) ) ;
#2803 = LINE ( 'NONE', #15632, #15852 ) ;
#2804 = EDGE_CURVE ( 'NONE', #2929, #19885, #4112, .T. ) ;
#2805 = CARTESIAN_POINT ( 'NONE',  ( 34.99999999999999289, 0.000000000000000000, 0.000000000000000000 ) ) ;
#2806 = EDGE_CURVE ( 'NONE', #590, #13152, #19557, .T. ) ;
#2807 = CARTESIAN_POINT ( 'NONE',  ( 45.00000000000000000, 272.9999999999999432, -5.249999999999973355 ) ) ;
#2808 = CARTESIAN_POINT ( 'NONE',  ( -281.8958543268122980, 268.8927021017106540, -145.9952621458756141 ) ) ;
#2809 = ORIENTED_EDGE ( 'NONE', *, *, #13318, .F. ) ;
#2810 = AXIS2_PLACEMENT_3D ( 'NONE', #15660, #12299, #2939 ) ;
#2811 = CARTESIAN_POINT ( 'NONE',  ( 281.4928932188133217, 267.7999999999999545, 150.1999999999999886 ) ) ;
#2812 = EDGE_CURVE ( 'NONE', #15145, #11487, #7202, .T. ) ;
#2813 = PRODUCT_DEFINITION ( 'UNKNOWN', '', #9676, #9534 ) ;
#2814 = DIRECTION ( 'NONE',  ( 0.000000000000000000, 0.000000000000000000, 1.000000000000000000 ) ) ;
#2815 = EDGE_CURVE ( 'NONE', #2924, #15992, #8977, .T. ) ;
#2816 = ORIENTED_EDGE ( 'NONE', *, *, #17131, .F. ) ;
#2817 = LINE ( 'NONE', #22858, #9012 ) ;
#2818 = ORIENTED_EDGE ( 'NONE', *, *, #22876, .T. ) ;
#2819 = DIRECTION ( 'NONE',  ( 1.000000000000000000, 0.000000000000000000, 0.000000000000000000 ) ) ;
#2820 = CARTESIAN_POINT ( 'NONE',  ( 89.00000000000000000, -149.9999999999996874, 129.9038105676659711 ) ) ;
#2821 = ORIENTED_EDGE ( 'NONE', *, *, #12730, .T. ) ;
#2822 = CARTESIAN_POINT ( 'NONE',  ( -24.19933745025247873, 6.487655866515821046, -145.0000000000000000 ) ) ;
#2823 = DIRECTION ( 'NONE',  ( 0.000000000000000000, 0.000000000000000000, 1.000000000000000000 ) ) ;
#2824 = PRODUCT ( 'socket head cap screw_iso_ISO 4762 M10 x 40 - 40N', 'socket head cap screw_iso_ISO 4762 M10 x 40 - 40N', '', ( #9407 ) ) ;
#2825 = PRESENTATION_LAYER_ASSIGNMENT (  '', '', ( #12137 ) ) ;
#2826 = CARTESIAN_POINT ( 'NONE',  ( -44.80746418436648071, -137.9031948627975908, 90.00000000000000000 ) ) ;
#2827 = DIRECTION ( 'NONE',  ( 0.000000000000000000, 1.224646799147346305E-16, 1.000000000000000000 ) ) ;
#2828 = CARTESIAN_POINT ( 'NONE',  ( 146.0000000000002274, -207.9450000000003627, -29.99999999999356604 ) ) ;
#2829 = DIRECTION ( 'NONE',  ( 0.000000000000000000, 0.000000000000000000, 1.000000000000000000 ) ) ;
#2830 = ORIENTED_EDGE ( 'NONE', *, *, #1765, .F. ) ;
#2831 = DIRECTION ( 'NONE',  ( 1.000000000000000000, 0.000000000000000000, 0.000000000000000000 ) ) ;
#2832 = DIRECTION ( 'NONE',  ( 0.000000000000000000, 1.177509268541832635E-16, -1.000000000000000000 ) ) ;
#2833 = VERTEX_POINT ( 'NONE', #14730 ) ;
#2834 = VERTEX_POINT ( 'NONE', #20366 ) ;
#2835 = CYLINDRICAL_SURFACE ( 'NONE', #4202, 24.99999999999998224 ) ;
#2836 = DIRECTION ( 'NONE',  ( 0.000000000000000000, -2.618450529776313049E-15, -1.000000000000000000 ) ) ;
#2837 = CARTESIAN_POINT ( 'NONE',  ( 20.00000000000000000, 0.000000000000000000, 200.0000000000000000 ) ) ;
#2838 = EDGE_CURVE ( 'NONE', #963, #1686, #23641, .T. ) ;
#2839 = EDGE_CURVE ( 'NONE', #12831, #22418, #21921, .T. ) ;
#2840 = CARTESIAN_POINT ( 'NONE',  ( 132.2605194320660189, 80.82189108482342021, 27.75096515221180837 ) ) ;
#2841 = EDGE_CURVE ( 'NONE', #15576, #12773, #20412, .T. ) ;
#2842 = CYLINDRICAL_SURFACE ( 'NONE', #16942, 2.649999999999971934 ) ;
#2843 = FACE_OUTER_BOUND ( 'NONE', #1269, .T. ) ;
#2844 = ORIENTED_EDGE ( 'NONE', *, *, #19085, .F. ) ;
#2845 = CARTESIAN_POINT ( 'NONE',  ( 67.35000000000002274, -112.6666666666666714, 3.000000000000001332 ) ) ;
#2846 = FACE_OUTER_BOUND ( 'NONE', #8329, .T. ) ;
#2847 = ORIENTED_EDGE ( 'NONE', *, *, #6643, .T. ) ;
#2848 = CARTESIAN_POINT ( 'NONE',  ( 155.0000000000000284, -209.9999999999996874, 30.00000000000648015 ) ) ;
#2849 = LINE ( 'NONE', #1285, #18056 ) ;
#2850 = CARTESIAN_POINT ( 'NONE',  ( 121.0905917848625251, -1085.936264790784435, -29.99999999999356604 ) ) ;
#2851 = CARTESIAN_POINT ( 'NONE',  ( -18.83879023463319058, -1016.516618489828488, -145.0000000000001421 ) ) ;
#2852 = CARTESIAN_POINT ( 'NONE',  ( -112.7436279071531828, 91.18044947428913360, -90.00000000000000000 ) ) ;
#2853 = CARTESIAN_POINT ( 'NONE',  ( -281.3488036478622121, 272.8335297745773005, 145.2489140339770017 ) ) ;
#2854 = AXIS2_PLACEMENT_3D ( 'NONE', #16273, #21451, #1634 ) ;
#2855 = ORIENTED_EDGE ( 'NONE', *, *, #20545, .T. ) ;
#2856 = AXIS2_PLACEMENT_3D ( 'NONE', #6457, #20954, #11818 ) ;
#2857 = ORIENTED_EDGE ( 'NONE', *, *, #13639, .F. ) ;
#2858 = CARTESIAN_POINT ( 'NONE',  ( -1.118033988749894458, 0.000000000000000000, 0.000000000000000000 ) ) ;
#2859 = CARTESIAN_POINT ( 'NONE',  ( 155.0000000000000284, -490.0000000000001137, -60.00000000000000000 ) ) ;
#2860 = ORIENTED_EDGE ( 'NONE', *, *, #10775, .F. ) ;
#2861 = AXIS2_PLACEMENT_3D ( 'NONE', #5285, #3576, #3224 ) ;
#2862 = ORIENTED_EDGE ( 'NONE', *, *, #6325, .T. ) ;
#2863 = CARTESIAN_POINT ( 'NONE',  ( -49.99999999999997158, -131.7994082814339833, 3.000000000000017764 ) ) ;
#2864 = CARTESIAN_POINT ( 'NONE',  ( 155.0000000000000568, -560.0000000000000000, 59.99999999999999289 ) ) ;
#2865 = ORIENTED_EDGE ( 'NONE', *, *, #6061, .T. ) ;
#2866 = CARTESIAN_POINT ( 'NONE',  ( -134.5482912860058207, -1076.952955187286989, -29.83126738556711288 ) ) ;
#2867 = EDGE_LOOP ( 'NONE', ( #2010, #8273 ) ) ;
#2868 = CIRCLE ( 'NONE', #5966, 5.249999999999949374 ) ;
#2869 = FACE_BOUND ( 'NONE', #4565, .T. ) ;
#2870 = PLANE ( 'NONE',  #21741 ) ;
#2871 = ORIENTED_EDGE ( 'NONE', *, *, #16274, .T. ) ;
#2872 = ORIENTED_EDGE ( 'NONE', *, *, #6862, .F. ) ;
#2873 = CARTESIAN_POINT ( 'NONE',  ( 0.000000000000000000, 0.000000000000000000, -90.00000000000000000 ) ) ;
#2874 = AXIS2_PLACEMENT_3D ( 'NONE', #20053, #18347, #8961 ) ;
#2875 = AXIS2_PLACEMENT_3D ( 'NONE', #4426, #11837, #21216 ) ;
#2876 = DIRECTION ( 'NONE',  ( 1.000000000000000000, 0.000000000000000000, 0.000000000000000000 ) ) ;
#2877 = CARTESIAN_POINT ( 'NONE',  ( 79.04925354955072692, 121.5574576620408322, 90.00000000000000000 ) ) ;
#2878 = DIRECTION ( 'NONE',  ( 1.110223024625155594E-14, 0.000000000000000000, -1.000000000000000000 ) ) ;
#2879 = ORIENTED_EDGE ( 'NONE', *, *, #13422, .F. ) ;
#2880 = FACE_BOUND ( 'NONE', #9684, .T. ) ;
#2881 = AXIS2_PLACEMENT_3D ( 'NONE', #14839, #8941, #16178 ) ;
#2882 = VERTEX_POINT ( 'NONE', #9889 ) ;
#2883 = EDGE_CURVE ( 'NONE', #11842, #20612, #7944, .T. ) ;
#2884 = CIRCLE ( 'NONE', #9085, 145.0000000000000284 ) ;
#2885 = ORIENTED_EDGE ( 'NONE', *, *, #22707, .F. ) ;
#2886 = CARTESIAN_POINT ( 'NONE',  ( -21.69904058246457268, -12.52399064369876669, -145.0000000000000000 ) ) ;
#2887 = ORIENTED_EDGE ( 'NONE', *, *, #18974, .F. ) ;
#2888 = DIRECTION ( 'NONE',  ( 0.000000000000000000, 1.000000000000000000, 0.000000000000000000 ) ) ;
#2889 = FACE_BOUND ( 'NONE', #11034, .T. ) ;
#2890 = EDGE_LOOP ( 'NONE', ( #21573, #13156, #5085, #231 ) ) ;
#2891 = EDGE_CURVE ( 'NONE', #13630, #11363, #5728, .T. ) ;
#2892 = VECTOR ( 'NONE', #19506, 1000.000000000000000 ) ;
#2893 = DIRECTION ( 'NONE',  ( 1.000000000000000000, 0.000000000000000000, -0.000000000000000000 ) ) ;
#2894 = EDGE_CURVE ( 'NONE', #4083, #13410, #9654, .T. ) ;
#2895 = CONTEXT_DEPENDENT_SHAPE_REPRESENTATION ( #11138, #20285 ) ;
#2896 = ORIENTED_EDGE ( 'NONE', *, *, #14175, .F. ) ;
#2897 = VECTOR ( 'NONE', #19054, 1000.000000000000000 ) ;
#2898 = DIRECTION ( 'NONE',  ( 0.000000000000000000, -2.618450529776326854E-15, -1.000000000000000000 ) ) ;
#2899 = CARTESIAN_POINT ( 'NONE',  ( 25.00000000000004974, -52.79999999999973426, 35.00000000000017764 ) ) ;
#2900 = EDGE_CURVE ( 'NONE', #10909, #18725, #8073, .T. ) ;
#2901 = CARTESIAN_POINT ( 'NONE',  ( -3.288228914120473245, 7.217643567644804747, -7.591235721156635030 ) ) ;
#2902 = CONICAL_SURFACE ( 'NONE', #1387, 2.055000000000001492, 0.7853981633974633780 ) ;
#2903 = CYLINDRICAL_SURFACE ( 'NONE', #16916, 5.249999999999942268 ) ;
#2904 = VERTEX_POINT ( 'NONE', #11845 ) ;
#2905 = LINE ( 'NONE', #869, #9612 ) ;
#2906 =( REPRESENTATION_RELATIONSHIP ('NONE','NONE', #10127, #5587 ) REPRESENTATION_RELATIONSHIP_WITH_TRANSFORMATION ( #3055 )SHAPE_REPRESENTATION_RELATIONSHIP( ) );
#2907 = PRODUCT_DEFINITION_SHAPE ( 'NONE', 'NONE',  #23864 ) ;
#2909 = ORIENTED_EDGE ( 'NONE', *, *, #22120, .T. ) ;
#2908 = ORIENTED_EDGE ( 'NONE', *, *, #18703, .F. ) ;
#2910 = DIRECTION ( 'NONE',  ( 6.123233995736766036E-17, 0.000000000000000000, -1.000000000000000000 ) ) ;
#2911 = FACE_OUTER_BOUND ( 'NONE', #15555, .T. ) ;
#2912 = CIRCLE ( 'NONE', #18734, 145.0000000000000284 ) ;
#2913 = CARTESIAN_POINT ( 'NONE',  ( 131.8485914335934410, 81.49210221337172300, -31.65735141704659128 ) ) ;
#2914 = DIRECTION ( 'NONE',  ( 0.000000000000000000, 0.000000000000000000, -1.000000000000000000 ) ) ;
#2915 = DIRECTION ( 'NONE',  ( -0.000000000000000000, -0.000000000000000000, 1.000000000000000000 ) ) ;
#2916 = LINE ( 'NONE', #14077, #12237 ) ;
#2917 = VERTEX_POINT ( 'NONE', #10012 ) ;
#2918 = CARTESIAN_POINT ( 'NONE',  ( -1.500000000000000000, 12.00000000000000000, 0.000000000000000000 ) ) ;
#2919 = ORIENTED_EDGE ( 'NONE', *, *, #13068, .T. ) ;
#2920 = EDGE_CURVE ( 'NONE', #1277, #23309, #20491, .T. ) ;
#2921 = CARTESIAN_POINT ( 'NONE',  ( 20.00000000000000000, -1000.000000000000000, -150.0000000000000000 ) ) ;
#2922 = DIRECTION ( 'NONE',  ( -1.000000000000000000, 0.000000000000000000, 0.000000000000000000 ) ) ;
#2923 = ITEM_DEFINED_TRANSFORMATION ( 'NONE', 'NONE', #20803,  #11210 ) ;
#2924 = VERTEX_POINT ( 'NONE', #11722 ) ;
#2925 = DIRECTION ( 'NONE',  ( -0.000000000000000000, 3.483493295888648978E-15, 1.000000000000000000 ) ) ;
#2926 = ORIENTED_EDGE ( 'NONE', *, *, #17865, .F. ) ;
#2927 = DIRECTION ( 'NONE',  ( 1.000000000000000000, 0.000000000000000000, 0.000000000000000000 ) ) ;
#2928 = FACE_OUTER_BOUND ( 'NONE', #3292, .T. ) ;
#2929 = VERTEX_POINT ( 'NONE', #19032 ) ;
#2930 = VECTOR ( 'NONE', #10906, 1000.000000000000000 ) ;
#2931 = ADVANCED_FACE ( 'NONE', ( #18787 ), #20773, .T. ) ;
#2932 = SURFACE_STYLE_USAGE ( .BOTH. , #15541 ) ;
#2933 = LINE ( 'NONE', #3298, #4940 ) ;
#2934 = EDGE_CURVE ( 'NONE', #21516, #7464, #17374, .T. ) ;
#2935 = DIRECTION ( 'NONE',  ( -1.110223024625157172E-14, 0.000000000000000000, -1.000000000000000000 ) ) ;
#2936 = AXIS2_PLACEMENT_3D ( 'NONE', #3907, #20324, #9729 ) ;
#2937 = CARTESIAN_POINT ( 'NONE',  ( -20.63749999999999929, 0.000000000000000000, 0.000000000000000000 ) ) ;
#2938 = DIRECTION ( 'NONE',  ( -0.000000000000000000, -0.000000000000000000, 1.000000000000000000 ) ) ;
#2939 = DIRECTION ( 'NONE',  ( 0.000000000000000000, 0.000000000000000000, 1.000000000000000000 ) ) ;
#2940 = EDGE_CURVE ( 'NONE', #4863, #7697, #8893, .T. ) ;
#2941 = ORIENTED_EDGE ( 'NONE', *, *, #10411, .F. ) ;
#2942 = CYLINDRICAL_SURFACE ( 'NONE', #22654, 2.500000000000000444 ) ;
#2943 = FACE_OUTER_BOUND ( 'NONE', #10466, .T. ) ;
#2944 = EDGE_CURVE ( 'NONE', #15856, #9608, #22362, .T. ) ;
#2945 = VECTOR ( 'NONE', #21265, 1000.000000000000000 ) ;
#2946 = ORIENTED_EDGE ( 'NONE', *, *, #14978, .T. ) ;
#2947 = ORIENTED_EDGE ( 'NONE', *, *, #20986, .F. ) ;
#2948 = LINE ( 'NONE', #16020, #14312 ) ;
#2949 = DIRECTION ( 'NONE',  ( 0.000000000000000000, 1.000000000000000000, 0.000000000000000000 ) ) ;
#2950 = AXIS2_PLACEMENT_3D ( 'NONE', #4962, #12382, #16079 ) ;
#2951 = CARTESIAN_POINT ( 'NONE',  ( -194.7500000000000284, -204.4690652294800657, 30.00000000000675726 ) ) ;
#2952 = CARTESIAN_POINT ( 'NONE',  ( 131.6954086522097214, 81.73939080771464205, 31.26048023074364579 ) ) ;
#2953 = CARTESIAN_POINT ( 'NONE',  ( 2.499999999999999556, 0.000000000000000000, 3.469446951953614189E-15 ) ) ;
#2954 = FACE_BOUND ( 'NONE', #11229, .T. ) ;
#2955 = ORIENTED_EDGE ( 'NONE', *, *, #20821, .F. ) ;
#2956 = FACE_OUTER_BOUND ( 'NONE', #16526, .T. ) ;
#2957 = CARTESIAN_POINT ( 'NONE',  ( 85.22886158240964960, -117.3074641843666370, 90.00000000000000000 ) ) ;
#2958 = B_SPLINE_CURVE_WITH_KNOTS ( 'NONE', 3,
 ( #8646, #68, #12662, #11072, #14561, #18391, #14803, #18177, #23715, #9122, #18277, #3546, #12546, #9004, #20205, #7170 ),
 .UNSPECIFIED., .F., .F.,
 ( 4, 2, 2, 2, 2, 2, 2, 4 ),
 ( 0.000000000000000000, 0.0009361184303669784889, 0.001404177645550537448, 0.001872236860734096623, 0.002340296075917655799, 0.002808355291101214540, 0.003276414506284773716, 0.003744473721468332891 ),
 .UNSPECIFIED. ) ;
#2959 = ADVANCED_FACE ( 'NONE', ( #14964 ), #13662, .F. ) ;
#2960 = PLANE ( 'NONE',  #8266 ) ;
#2961 = ORIENTED_EDGE ( 'NONE', *, *, #18419, .T. ) ;
#2962 = SURFACE_SIDE_STYLE ('',( #19510 ) ) ;
#2963 = CARTESIAN_POINT ( 'NONE',  ( 34.99999999999999289, 90.00000000000000000, 3.000000000000000000 ) ) ;
#2964 = CARTESIAN_POINT ( 'NONE',  ( 171.6502151485109380, 95.33502053007563859, 32.50000000000675726 ) ) ;
#2965 = CARTESIAN_POINT ( 'NONE',  ( -288.2000000000013529, -89.99999999999897682, 21.68333333333335844 ) ) ;
#2966 = EDGE_CURVE ( 'NONE', #2924, #10594, #15323, .T. ) ;
#2968 = VECTOR ( 'NONE', #17545, 1000.000000000000000 ) ;
#2967 = CARTESIAN_POINT ( 'NONE',  ( 5.000000000000002665, 0.000000000000000000, -2.700000000000000622 ) ) ;
#2969 = DIRECTION ( 'NONE',  ( 0.000000000000000000, -1.000000000000000000, 0.000000000000000000 ) ) ;
#2970 = CIRCLE ( 'NONE', #6066, 2.649999999999975486 ) ;
#2971 = CARTESIAN_POINT ( 'NONE',  ( -283.1682701916307110, 271.9268706878666535, 145.6222583006965863 ) ) ;
#2972 = EDGE_LOOP ( 'NONE', ( #19259, #16489, #3704, #1292 ) ) ;
#2974 = ORIENTED_EDGE ( 'NONE', *, *, #4137, .T. ) ;
#2973 = EDGE_CURVE ( 'NONE', #6750, #6295, #18922, .T. ) ;
#2975 = CARTESIAN_POINT ( 'NONE',  ( -281.1815513148989112, 268.5095819834011763, -147.0873946496625422 ) ) ;
#2976 = CARTESIAN_POINT ( 'NONE',  ( 280.6212670861564220, 269.5502846751310244, 146.3405375976306857 ) ) ;
#2977 = ADVANCED_FACE ( 'NONE', ( #22536 ), #17691, .T. ) ;
#2978 = ORIENTED_EDGE ( 'NONE', *, *, #8640, .T. ) ;
#2979 = DIRECTION ( 'NONE',  ( 2.238759164535664589E-46, 3.469446951953614189E-15, 1.000000000000000000 ) ) ;
#2980 = DIRECTION ( 'NONE',  ( -1.000000000000000000, -0.000000000000000000, -0.000000000000000000 ) ) ;
#2981 = CIRCLE ( 'NONE', #18802, 2.650000000000041211 ) ;
#2982 = VERTEX_POINT ( 'NONE', #18663 ) ;
#2983 = CARTESIAN_POINT ( 'NONE',  ( 281.4928932188134354, -129.2000000000000455, -152.4000000000013131 ) ) ;
#2984 = DIRECTION ( 'NONE',  ( 0.000000000000000000, 0.000000000000000000, 1.000000000000000000 ) ) ;
#2985 = ORIENTED_EDGE ( 'NONE', *, *, #3854, .F. ) ;
#2986 = DIRECTION ( 'NONE',  ( -0.000000000000000000, -0.000000000000000000, 1.000000000000000000 ) ) ;
#2987 = CIRCLE ( 'NONE', #12307, 2.649999999999985700 ) ;
#2988 = CIRCLE ( 'NONE', #16132, 2.055000000000001492 ) ;
#2989 = VERTEX_POINT ( 'NONE', #20978 ) ;
#2990 = DIRECTION ( 'NONE',  ( 1.000000000000000000, 0.000000000000000000, 0.000000000000000000 ) ) ;
#2991 = CARTESIAN_POINT ( 'NONE',  ( 1.500000000000000000, 12.00000000000000000, 0.000000000000000000 ) ) ;
#2992 = VERTEX_POINT ( 'NONE', #13412 ) ;
#2993 = EDGE_LOOP ( 'NONE', ( #20270, #13924, #8741, #2493 ) ) ;
#2994 = CARTESIAN_POINT ( 'NONE',  ( 133.9567665909160326, 77.97815834559297343, -28.74099766568597758 ) ) ;
#2995 = CARTESIAN_POINT ( 'NONE',  ( -39.99999999999999289, 100.0000000000000000, -114.9999999999999574 ) ) ;
#2996 = EDGE_CURVE ( 'NONE', #6747, #442, #7706, .T. ) ;
#2997 = DIRECTION ( 'NONE',  ( -0.000000000000000000, -0.000000000000000000, 1.000000000000000000 ) ) ;
#2998 = CARTESIAN_POINT ( 'NONE',  ( 281.4928932188134354, -127.0000000000000568, -147.2000000000013245 ) ) ;
#2999 = VECTOR ( 'NONE', #7777, 1000.000000000000000 ) ;
#3000 = CARTESIAN_POINT ( 'NONE',  ( 194.7499999999997442, -801.0618695410399823, 30.00000000000675726 ) ) ;
#3001 = ORIENTED_EDGE ( 'NONE', *, *, #10546, .T. ) ;
#3002 = ADVANCED_FACE ( 'NONE', ( #16874 ), #20726, .F. ) ;
#3003 = CIRCLE ( 'NONE', #14595, 1.500000000000001332 ) ;
#3004 = CARTESIAN_POINT ( 'NONE',  ( -129.2206655591611764, -1072.408698320350140, -32.05499999999356930 ) ) ;
#3005 = AXIS2_PLACEMENT_3D ( 'NONE', #7570, #5878, #2007 ) ;
#3006 = VECTOR ( 'NONE', #22601, 1000.000000000000000 ) ;
#3007 = CIRCLE ( 'NONE', #23458, 2.649999999999999467 ) ;
#3008 = ORIENTED_EDGE ( 'NONE', *, *, #4358, .T. ) ;
#3009 = EDGE_CURVE ( 'NONE', #10015, #9003, #20055, .T. ) ;
#3010 = VERTEX_POINT ( 'NONE', #579 ) ;
#3011 = CARTESIAN_POINT ( 'NONE',  ( -15.25450579711302623, -19.87456868343288363, -145.0000000000000000 ) ) ;
#3012 = ORIENTED_EDGE ( 'NONE', *, *, #17601, .F. ) ;
#3013 = CARTESIAN_POINT ( 'NONE',  ( 6.484173630542770184, 4.916614646782027087, -7.642786413619098163 ) ) ;
#3014 = FACE_BOUND ( 'NONE', #15228, .T. ) ;
#3015 = VERTEX_POINT ( 'NONE', #10497 ) ;
#3016 = PRODUCT_DEFINITION_SHAPE ( 'NONE', 'NONE',  #23807 ) ;
#3017 = CONICAL_SURFACE ( 'NONE', #18819, 2.055000000000001492, 0.7853981633974633780 ) ;
#3018 = CARTESIAN_POINT ( 'NONE',  ( -136.3245111336058812, -1073.760768802673056, 27.75040112528352765 ) ) ;
#3019 = CARTESIAN_POINT ( 'NONE',  ( 102.3500000000000227, 35.00000000000000000, 3.000000000000000000 ) ) ;
#3020 = AXIS2_PLACEMENT_3D ( 'NONE', #4196, #8428, #20989 ) ;
#3021 = ORIENTED_EDGE ( 'NONE', *, *, #9056, .T. ) ;
#3022 = VECTOR ( 'NONE', #33, 1000.000000000000000 ) ;
#3023 = PLANE ( 'NONE',  #7333 ) ;
#3024 = FACE_BOUND ( 'NONE', #16999, .T. ) ;
#3025 = AXIS2_PLACEMENT_3D ( 'NONE', #2381, #9766, #17122 ) ;
#3026 = LINE ( 'NONE', #10557, #14282 ) ;
#3027 = FACE_OUTER_BOUND ( 'NONE', #20509, .T. ) ;
#3028 = EDGE_LOOP ( 'NONE', ( #16211, #16269, #12851, #22501 ) ) ;
#3029 = CARTESIAN_POINT ( 'NONE',  ( 194.7499999999997726, -801.0618695410399823, 27.50000000000675371 ) ) ;
#3030 =( LENGTH_UNIT ( ) NAMED_UNIT ( * ) SI_UNIT ( .MILLI., .METRE. ) );
#3031 = EDGE_CURVE ( 'NONE', #21305, #6640, #16542, .T. ) ;
#3033 = ORIENTED_EDGE ( 'NONE', *, *, #15822, .F. ) ;
#3032 = ORIENTED_EDGE ( 'NONE', *, *, #21249, .F. ) ;
#3034 = ADVANCED_FACE ( 'NONE', ( #17712 ), #16030, .F. ) ;
#3035 = VECTOR ( 'NONE', #22982, 1000.000000000000000 ) ;
#3036 = DIRECTION ( 'NONE',  ( -3.469446951953613794E-15, 3.469446951953612611E-15, 1.000000000000000000 ) ) ;
#3037 = CIRCLE ( 'NONE', #10027, 4.171999999999999709 ) ;
#3038 = CARTESIAN_POINT ( 'NONE',  ( 281.4928932188134354, -129.2000000000000455, -177.2000000000013529 ) ) ;
#3039 = DIRECTION ( 'NONE',  ( -0.000000000000000000, -0.000000000000000000, 1.000000000000000000 ) ) ;
#3040 = CIRCLE ( 'NONE', #12737, 25.00000000000000000 ) ;
#3041 = AXIS2_PLACEMENT_3D ( 'NONE', #19482, #13991, #4770 ) ;
#3042 = PRESENTATION_LAYER_ASSIGNMENT (  '', '', ( #13888 ) ) ;
#3043 = AXIS2_PLACEMENT_3D ( 'NONE', #3870, #18482, #16682 ) ;
#3044 = FACE_OUTER_BOUND ( 'NONE', #6003, .T. ) ;
#3045 = DIRECTION ( 'NONE',  ( 0.000000000000000000, 0.000000000000000000, 1.000000000000000000 ) ) ;
#3046 = CARTESIAN_POINT ( 'NONE',  ( -281.0927021017107563, 269.6958543268121957, -145.4976310729377929 ) ) ;
#3047 = ORIENTED_EDGE ( 'NONE', *, *, #12437, .T. ) ;
#3048 = ADVANCED_FACE ( 'NONE', ( #17950, #4912, #17585 ), #14237, .F. ) ;
#3049 =( REPRESENTATION_RELATIONSHIP ('NONE','NONE', #10127, #14711 ) REPRESENTATION_RELATIONSHIP_WITH_TRANSFORMATION ( #22500 )SHAPE_REPRESENTATION_RELATIONSHIP( ) );
#3050 = DIRECTION ( 'NONE',  ( 0.000000000000000000, 0.000000000000000000, -1.000000000000000000 ) ) ;
#3051 = ORIENTED_EDGE ( 'NONE', *, *, #20882, .F. ) ;
#3052 = CIRCLE ( 'NONE', #23099, 4.250000000000000000 ) ;
#3053 = CARTESIAN_POINT ( 'NONE',  ( 100.0000000000000000, 249.9999999999999716, 125.0000000000000284 ) ) ;
#3054 = SURFACE_STYLE_FILL_AREA ( #8512 ) ;
#3055 = ITEM_DEFINED_TRANSFORMATION ( 'NONE', 'NONE', #1136,  #11210 ) ;
#3056 = ORIENTED_EDGE ( 'NONE', *, *, #23066, .F. ) ;
#3057 = DIRECTION ( 'NONE',  ( -0.000000000000000000, -0.000000000000000000, 1.000000000000000000 ) ) ;
#3058 = VERTEX_POINT ( 'NONE', #4789 ) ;
#3059 = CARTESIAN_POINT ( 'NONE',  ( 5.000000000000000000, 4.685197434473814759, -5.637851296924623057E-15 ) ) ;
#3060 = DIRECTION ( 'NONE',  ( -1.000000000000000000, 0.000000000000000000, 0.000000000000000000 ) ) ;
#3062 = AXIS2_PLACEMENT_3D ( 'NONE', #5301, #21831, #5534 ) ;
#3061 = AXIS2_PLACEMENT_3D ( 'NONE', #4864, #23575, #13968 ) ;
#3063 = ORIENTED_EDGE ( 'NONE', *, *, #9786, .T. ) ;
#3064 = DIRECTION ( 'NONE',  ( 1.000000000000000000, 3.495664435217746592E-15, -0.000000000000000000 ) ) ;
#3065 = CONICAL_SURFACE ( 'NONE', #4991, 4.057500000000000107, 1.047197551196593857 ) ;
#3066 = CARTESIAN_POINT ( 'NONE',  ( 2.500000000000000000, 2.357898499370432166, -2.385244779468109755E-15 ) ) ;
#3067 = VECTOR ( 'NONE', #10793, 1000.000000000000000 ) ;
#3068 = VECTOR ( 'NONE', #3169, 1000.000000000000000 ) ;
#3069 = AXIS2_PLACEMENT_3D ( 'NONE', #19767, #10383, #15579 ) ;
#3070 = CARTESIAN_POINT ( 'NONE',  ( -7.497491405671719455, 144.8060344827586334, -2.775557561562891351E-14 ) ) ;
#3071 = FACE_OUTER_BOUND ( 'NONE', #15603, .T. ) ;
#3072 = LINE ( 'NONE', #10339, #13022 ) ;
#3073 = CARTESIAN_POINT ( 'NONE',  ( 0.000000000000000000, 8.878689293818310074E-16, -6.500000000000000888 ) ) ;
#3074 = DIRECTION ( 'NONE',  ( 0.000000000000000000, 0.000000000000000000, 1.000000000000000000 ) ) ;
#3075 = EDGE_LOOP ( 'NONE', ( #16565, #17357, #19371, #4735, #9836, #18694 ) ) ;
#3076 = EDGE_CURVE ( 'NONE', #21515, #14004, #19612, .T. ) ;
#3077 = DIRECTION ( 'NONE',  ( -1.000000000000000000, 1.408839003528726857E-14, 6.982962677686266711E-15 ) ) ;
#3078 = CARTESIAN_POINT ( 'NONE',  ( -4.197312064133472020, -0.8182229787990021874, -3.502518405183886685 ) ) ;
#3079 = ORIENTED_EDGE ( 'NONE', *, *, #12259, .T. ) ;
#3080 = VERTEX_POINT ( 'NONE', #13894 ) ;
#3081 = CARTESIAN_POINT ( 'NONE',  ( -146.0000000000001137, -204.4690652294807478, 27.94500000000641649 ) ) ;
#3082 = DIRECTION ( 'NONE',  ( -0.000000000000000000, -0.000000000000000000, 1.000000000000000000 ) ) ;
#3083 = AXIS2_PLACEMENT_3D ( 'NONE', #8949, #5185, #16307 ) ;
#3084 = VECTOR ( 'NONE', #7877, 1000.000000000000000 ) ;
#3085 = ADVANCED_FACE ( 'NONE', ( #2846 ), #15915, .T. ) ;
#3086 = EDGE_CURVE ( 'NONE', #21146, #19747, #19634, .T. ) ;
#3087 = VECTOR ( 'NONE', #7219, 1000.000000000000000 ) ;
#3088 = DIRECTION ( 'NONE',  ( -1.000000000000000000, -0.000000000000000000, -0.000000000000000000 ) ) ;
#3089 = VECTOR ( 'NONE', #9119, 1000.000000000000000 ) ;
#3090 = CARTESIAN_POINT ( 'NONE',  ( 131.7919310846380654, 81.58367163796999932, 28.47118012353583794 ) ) ;
#3091 = FACE_OUTER_BOUND ( 'NONE', #8718, .T. ) ;
#3092 = ORIENTED_EDGE ( 'NONE', *, *, #9070, .F. ) ;
#3093 = CARTESIAN_POINT ( 'NONE',  ( -287.4000000000014552, -129.2000000000000455, -146.4928932188134070 ) ) ;
#3094 = VERTEX_POINT ( 'NONE', #2746 ) ;
#3095 = DIRECTION ( 'NONE',  ( -0.000000000000000000, -0.000000000000000000, 1.000000000000000000 ) ) ;
#3097 = EDGE_CURVE ( 'NONE', #16162, #21528, #2541, .T. ) ;
#3096 = CARTESIAN_POINT ( 'NONE',  ( -3.333333333333332149, -2.694301256218264218, -3.300726591567082036 ) ) ;
#3098 = CARTESIAN_POINT ( 'NONE',  ( -175.1609685624536041, -1088.719770019218913, 32.50000000000675726 ) ) ;
#3099 = EDGE_LOOP ( 'NONE', ( #14042, #21270 ) ) ;
#3100 = CARTESIAN_POINT ( 'NONE',  ( -34.75000000000005684, 100.0000000000000000, 125.0000000000000000 ) ) ;
#3101 = DIRECTION ( 'NONE',  ( -0.9423651898111408132, -0.3345860861306287348, 6.982962677686266711E-15 ) ) ;
#3102 = FACE_OUTER_BOUND ( 'NONE', #22549, .T. ) ;
#3103 = DIRECTION ( 'NONE',  ( -1.000000000000000000, 1.408839003528726857E-14, 6.982962677686266711E-15 ) ) ;
#3104 = LINE ( 'NONE', #3480, #11493 ) ;
#3105 = CARTESIAN_POINT ( 'NONE',  ( -5.560781378645573980, 0.000000000000000000, -4.000000000000000000 ) ) ;
#3106 = DIRECTION ( 'NONE',  ( 1.000000000000000000, 0.000000000000000000, 0.000000000000000000 ) ) ;
#3107 = DIRECTION ( 'NONE',  ( 0.000000000000000000, 0.000000000000000000, -1.000000000000000000 ) ) ;
#3108 = AXIS2_PLACEMENT_3D ( 'NONE', #16381, #1747, #18295 ) ;
#3109 = EDGE_LOOP ( 'NONE', ( #20326, #20107, #3159, #5201, #14814, #19397 ) ) ;
#3110 = VERTEX_POINT ( 'NONE', #6364 ) ;
#3111 = CARTESIAN_POINT ( 'NONE',  ( 0.000000000000000000, -1000.000000000000000, 124.9999999999998579 ) ) ;
#3112 = CARTESIAN_POINT ( 'NONE',  ( 281.1815513148990817, 268.5095819834012332, 147.0873946496626274 ) ) ;
#3113 = VERTEX_POINT ( 'NONE', #8546 ) ;
#3114 = DIRECTION ( 'NONE',  ( 0.000000000000000000, 0.000000000000000000, 1.000000000000000000 ) ) ;
#3115 = DIRECTION ( 'NONE',  ( -0.5000000000000051070, 1.060575238724903217E-16, -0.8660254037844355990 ) ) ;
#3116 = EDGE_CURVE ( 'NONE', #7326, #7198, #10611, .T. ) ;
#3117 = EDGE_LOOP ( 'NONE', ( #17465, #3540, #13345, #22736 ) ) ;
#3118 = CYLINDRICAL_SURFACE ( 'NONE', #11040, 2.199999999999979750 ) ;
#3119 = EDGE_CURVE ( 'NONE', #3718, #13209, #8415, .T. ) ;
#3120 = DIRECTION ( 'NONE',  ( -1.000000000000000000, 0.000000000000000000, 0.000000000000000000 ) ) ;
#3121 = ORIENTED_EDGE ( 'NONE', *, *, #14762, .F. ) ;
#3122 = EDGE_CURVE ( 'NONE', #6763, #17109, #2315, .T. ) ;
#3123 = CARTESIAN_POINT ( 'NONE',  ( -134.5892462183201701, -1076.881310361371789, -29.34624901867148949 ) ) ;
#3124 = SHAPE_REPRESENTATION ( 'motor', ( #11210 ), #7665 ) ;
#3125 = ADVANCED_FACE ( 'NONE', ( #11971 ), #23250, .T. ) ;
#3126 = ORIENTED_EDGE ( 'NONE', *, *, #9156, .T. ) ;
#3127 = EDGE_CURVE ( 'NONE', #16976, #14993, #12202, .T. ) ;
#3128 = CARTESIAN_POINT ( 'NONE',  ( -4.154094228333736538, -2.398367420967545627, -3.721909803043222276 ) ) ;
#3129 = EDGE_CURVE ( 'NONE', #13899, #4603, #19279, .T. ) ;
#3130 = CARTESIAN_POINT ( 'NONE',  ( 112.7436279071518612, 91.18044947429076785, 90.00000000000000000 ) ) ;
#3131 = VERTEX_POINT ( 'NONE', #17477 ) ;
#3132 = EDGE_LOOP ( 'NONE', ( #3290, #805, #21657, #11861, #5062, #18814 ) ) ;
#3133 = CARTESIAN_POINT ( 'NONE',  ( 134.0925202534287166, 77.74453171555532549, -30.66034227022097625 ) ) ;
#3134 = PRODUCT_DEFINITION_SHAPE ( 'NONE', 'NONE',  #23839 ) ;
#3135 = DIRECTION ( 'NONE',  ( 6.123233995736766036E-17, 0.000000000000000000, 1.000000000000000000 ) ) ;
#3136 = DIRECTION ( 'NONE',  ( 0.000000000000000000, -0.000000000000000000, 1.000000000000000000 ) ) ;
#3137 = DIRECTION ( 'NONE',  ( 1.000000000000000000, 0.000000000000000000, 0.000000000000000000 ) ) ;
#3138 = CARTESIAN_POINT ( 'NONE',  ( 285.2000000000013529, -127.0000000000000568, 0.000000000000000000 ) ) ;
#3139 = VERTEX_POINT ( 'NONE', #19507 ) ;
#3140 = FACE_OUTER_BOUND ( 'NONE', #430, .T. ) ;
#3141 = ORIENTED_EDGE ( 'NONE', *, *, #14682, .T. ) ;
#3142 = VERTEX_POINT ( 'NONE', #921 ) ;
#3143 = DIRECTION ( 'NONE',  ( -1.000000000000000000, 3.495664435217746592E-15, -0.000000000000000000 ) ) ;
#3144 = ORIENTED_EDGE ( 'NONE', *, *, #2061, .F. ) ;
#3145 = FACE_OUTER_BOUND ( 'NONE', #6804, .T. ) ;
#3146 = EDGE_LOOP ( 'NONE', ( #10561, #13581, #1185, #10583 ) ) ;
#3147 = EDGE_CURVE ( 'NONE', #4706, #6149, #16156, .T. ) ;
#3148 = EDGE_CURVE ( 'NONE', #16779, #14572, #23143, .T. ) ;
#3149 = ORIENTED_EDGE ( 'NONE', *, *, #9898, .T. ) ;
#3150 = CYLINDRICAL_SURFACE ( 'NONE', #10428, 2.500000000000002220 ) ;
#3151 = CARTESIAN_POINT ( 'NONE',  ( -280.0627656775836840, 269.9999999999999432, 145.1452901038202015 ) ) ;
#3152 = DIRECTION ( 'NONE',  ( 1.000000000000000000, 0.000000000000000000, 0.000000000000000000 ) ) ;
#3153 = CARTESIAN_POINT ( 'NONE',  ( 155.0000000000000284, -209.9999999999996874, 32.50000000000648015 ) ) ;
#3154 = LINE ( 'NONE', #18141, #3403 ) ;
#3155 = VERTEX_POINT ( 'NONE', #1526 ) ;
#3156 = CARTESIAN_POINT ( 'NONE',  ( 40.00000000000000000, 100.0000000000000000, 150.2000000000009550 ) ) ;
#3157 = VECTOR ( 'NONE', #13548, 1000.000000000000114 ) ;
#3159 = ORIENTED_EDGE ( 'NONE', *, *, #18614, .T. ) ;
#3158 = ORIENTED_EDGE ( 'NONE', *, *, #19479, .F. ) ;
#3160 = DIRECTION ( 'NONE',  ( 1.000000000000000000, 2.832769448823979947E-16, -2.832769448823989808E-16 ) ) ;
#3161 = DIRECTION ( 'NONE',  ( -0.7232617928448825673, 0.6905739489807055653, 6.982962677686266711E-15 ) ) ;
#3162 = DIRECTION ( 'NONE',  ( 0.000000000000000000, -1.000000000000000000, 1.287488025362403787E-15 ) ) ;
#3163 = DIRECTION ( 'NONE',  ( 0.000000000000000000, -0.5000000000000009992, -0.8660254037844380415 ) ) ;
#3164 = CARTESIAN_POINT ( 'NONE',  ( 194.7500000000001990, -210.0000000000003411, -29.99999999999322498 ) ) ;
#3165 = EDGE_LOOP ( 'NONE', ( #12116, #5371, #23614, #16895 ) ) ;
#3166 = DIRECTION ( 'NONE',  ( 0.000000000000000000, -0.5000000000000012212, -0.8660254037844380415 ) ) ;
#3167 = ORIENTED_EDGE ( 'NONE', *, *, #23772, .F. ) ;
#3168 = PLANE ( 'NONE',  #4606 ) ;
#3169 = DIRECTION ( 'NONE',  ( 0.000000000000000000, 3.483493295888648978E-15, 1.000000000000000000 ) ) ;
#3170 = ORIENTED_EDGE ( 'NONE', *, *, #14229, .F. ) ;
#3171 = AXIS2_PLACEMENT_3D ( 'NONE', #7719, #587, #18797 ) ;
#3172 = CARTESIAN_POINT ( 'NONE',  ( -0.5636800770129166693, -4.293361309317430319, -3.531542292955206275 ) ) ;
#3173 = ORIENTED_EDGE ( 'NONE', *, *, #8892, .F. ) ;
#3174 = CARTESIAN_POINT ( 'NONE',  ( -128.5309343563509969, 86.63037569149948069, -32.24903484778816676 ) ) ;
#3175 = CARTESIAN_POINT ( 'NONE',  ( -31.74999999999995737, 0.000000000000000000, 0.000000000000000000 ) ) ;
#3176 = ORIENTED_EDGE ( 'NONE', *, *, #12128, .F. ) ;
#3177 = SURFACE_STYLE_USAGE ( .BOTH. , #16004 ) ;
#3178 = CARTESIAN_POINT ( 'NONE',  ( 0.000000000000000000, -1.178949249685218081, -2.041999999999998039 ) ) ;
#3179 = CARTESIAN_POINT ( 'NONE',  ( 0.000000000000000000, 0.000000000000000000, -125.0000000000000000 ) ) ;
#3180 = DIRECTION ( 'NONE',  ( -0.9423651898111408132, -0.3345860861306287348, 6.982962677686266711E-15 ) ) ;
#3181 = DIRECTION ( 'NONE',  ( 5.758888509154132365E-17, 0.7071067811865489050, 0.7071067811865462405 ) ) ;
#3182 = CARTESIAN_POINT ( 'NONE',  ( -112.7436279071525433, -91.18044947428992941, 90.00000000000000000 ) ) ;
#3183 = ORIENTED_EDGE ( 'NONE', *, *, #14869, .F. ) ;
#3184 = DIRECTION ( 'NONE',  ( -1.000000000000000000, 0.000000000000000000, 0.000000000000000000 ) ) ;
#3185 = ORIENTED_EDGE ( 'NONE', *, *, #10970, .T. ) ;
#3186 = CIRCLE ( 'NONE', #2026, 25.00000000000000000 ) ;
#3187 = ORIENTED_EDGE ( 'NONE', *, *, #3737, .F. ) ;
#3188 = CARTESIAN_POINT ( 'NONE',  ( -146.0000000000001421, -206.5240652294807546, 30.00000000000641620 ) ) ;
#3189 = DIRECTION ( 'NONE',  ( 3.736327486719275871E-16, -1.000000000000000000, 3.469446951953613794E-15 ) ) ;
#3190 = EDGE_CURVE ( 'NONE', #23656, #7557, #4578, .T. ) ;
#3191 = CARTESIAN_POINT ( 'NONE',  ( -37.61698748598617925, 140.0355749532209870, -2.775557561562891351E-14 ) ) ;
#3192 = CYLINDRICAL_SURFACE ( 'NONE', #18803, 5.249999999999973355 ) ;
#3193 = CARTESIAN_POINT ( 'NONE',  ( -14.99999999999998934, -1.734723475976807094E-15, -10.00000000000000000 ) ) ;
#3194 = ORIENTED_EDGE ( 'NONE', *, *, #6533, .T. ) ;
#3195 = FACE_OUTER_BOUND ( 'NONE', #22778, .T. ) ;
#3196 = ORIENTED_EDGE ( 'NONE', *, *, #18555, .F. ) ;
#3197 = EDGE_CURVE ( 'NONE', #15650, #11272, #16145, .T. ) ;
#3198 = CARTESIAN_POINT ( 'NONE',  ( -4.000000000000000000, -2.309401076758512694, -3.433295621305382461 ) ) ;
#3199 = DIRECTION ( 'NONE',  ( -0.7232617928448825673, 0.6905739489807055653, 6.982962677686266711E-15 ) ) ;
#3200 = COLOUR_RGB ( '',0.8941176470588234615, 0.8941176470588234615, 0.8941176470588234615 ) ;
#3201 = DIRECTION ( 'NONE',  ( 1.000000000000000000, -0.000000000000000000, -0.000000000000000000 ) ) ;
#3202 = EDGE_CURVE ( 'NONE', #2989, #7088, #11950, .T. ) ;
#3203 = VERTEX_POINT ( 'NONE', #23725 ) ;
#3204 = CARTESIAN_POINT ( 'NONE',  ( 90.00000000000000000, 75.00000000000000000, 0.000000000000000000 ) ) ;
#3205 = CARTESIAN_POINT ( 'NONE',  ( 4.406842699996126989, -6.115962218725295330, -6.291760732204942919E-15 ) ) ;
#3206 = CARTESIAN_POINT ( 'NONE',  ( 93.00000000000000000, 3.000000000000280220, 129.9038105676659711 ) ) ;
#3207 = DIRECTION ( 'NONE',  ( -0.000000000000000000, -0.000000000000000000, 1.000000000000000000 ) ) ;
#3208 = CARTESIAN_POINT ( 'NONE',  ( 2.500000000000002220, 2.357898499370434386, -3.469446951953614189E-15 ) ) ;
#3209 = EDGE_CURVE ( 'NONE', #4361, #20959, #18133, .T. ) ;
#3210 = DIRECTION ( 'NONE',  ( 0.000000000000000000, 0.000000000000000000, -1.000000000000000000 ) ) ;
#3211 = LINE ( 'NONE', #1645, #17103 ) ;
#3212 = ORIENTED_EDGE ( 'NONE', *, *, #2061, .T. ) ;
#3213 = ORIENTED_EDGE ( 'NONE', *, *, #12473, .F. ) ;
#3214 = DIRECTION ( 'NONE',  ( 0.6964005597823107463, -0.7176533009294141507, 6.982962677686266711E-15 ) ) ;
#3215 = CARTESIAN_POINT ( 'NONE',  ( 145.0000000000000284, -500.0000000000000000, 30.00000000000001421 ) ) ;
#3216 = ORIENTED_EDGE ( 'NONE', *, *, #10905, .T. ) ;
#3217 = VECTOR ( 'NONE', #15097, 1000.000000000000000 ) ;
#3218 = PRODUCT ( 'motor', 'motor', '', ( #7579 ) ) ;
#3219 = CARTESIAN_POINT ( 'NONE',  ( 70.00000000000000000, -87.33333333333332860, 0.000000000000000000 ) ) ;
#3221 = AXIS2_PLACEMENT_3D ( 'NONE', #11449, #13391, #1992 ) ;
#3220 = DIRECTION ( 'NONE',  ( 0.000000000000000000, 0.000000000000000000, 1.000000000000000000 ) ) ;
#3222 = EDGE_LOOP ( 'NONE', ( #3855, #5994 ) ) ;
#3223 = B_SPLINE_CURVE_WITH_KNOTS ( 'NONE', 3,
 ( #19930, #16436, #23786, #21986, #20161, #18947, #17277, #20517 ),
 .UNSPECIFIED., .F., .F.,
 ( 4, 2, 2, 4 ),
 ( 2.465131517075058656E-07, 0.001183067374689851080, 0.001774477805458923299, 0.002365888236227995517 ),
 .UNSPECIFIED. ) ;
#3224 = DIRECTION ( 'NONE',  ( -1.000000000000000000, 0.000000000000000000, 0.000000000000000000 ) ) ;
#3225 = CARTESIAN_POINT ( 'NONE',  ( -146.0000000000004832, -494.4690652294800657, -27.94499999999356632 ) ) ;
#3226 = ORIENTED_EDGE ( 'NONE', *, *, #17108, .F. ) ;
#3227 = CARTESIAN_POINT ( 'NONE',  ( -135.7102838464028878, -1074.884883977197887, -27.49999999999352696 ) ) ;
#3228 = EDGE_LOOP ( 'NONE', ( #4081, #20543 ) ) ;
#3229 = ADVANCED_BREP_SHAPE_REPRESENTATION ( '', ( #12677, #11210 ), #1906 ) ;
#3230 = FACE_BOUND ( 'NONE', #19593, .T. ) ;
#3231 =( REPRESENTATION_RELATIONSHIP ('NONE','NONE', #10127, #5587 ) REPRESENTATION_RELATIONSHIP_WITH_TRANSFORMATION ( #14901 )SHAPE_REPRESENTATION_RELATIONSHIP( ) );
#3232 = CARTESIAN_POINT ( 'NONE',  ( 5.000000000000000888, 0.000000000000000000, 0.000000000000000000 ) ) ;
#3233 = ORIENTED_EDGE ( 'NONE', *, *, #17686, .T. ) ;
#3234 = ORIENTED_EDGE ( 'NONE', *, *, #21969, .F. ) ;
#3235 = CARTESIAN_POINT ( 'NONE',  ( 132.8404720734533555, 79.86494211668886578, -32.49999999999351985 ) ) ;
#3236 = MECHANICAL_DESIGN_GEOMETRIC_PRESENTATION_REPRESENTATION (  '', ( #6329 ), #19822 ) ;
#3237 = EDGE_CURVE ( 'NONE', #15299, #12940, #9016, .T. ) ;
#3238 =( LENGTH_UNIT ( ) NAMED_UNIT ( * ) SI_UNIT ( .MILLI., .METRE. ) );
#3239 = DIRECTION ( 'NONE',  ( 0.000000000000000000, 0.000000000000000000, 1.000000000000000000 ) ) ;
#3240 = VECTOR ( 'NONE', #22984, 1000.000000000000000 ) ;
#3241 = EDGE_CURVE ( 'NONE', #5473, #13502, #5147, .T. ) ;
#3242 = DIRECTION ( 'NONE',  ( 0.000000000000000000, 0.000000000000000000, -1.000000000000000000 ) ) ;
#3243 = AXIS2_PLACEMENT_3D ( 'NONE', #3253, #1575, #17998 ) ;
#3244 = CARTESIAN_POINT ( 'NONE',  ( 59.99999999999998579, -59.79999999999999005, 5.199999999999994849 ) ) ;
#3245 = ADVANCED_FACE ( 'NONE', ( #3451 ), #3322, .F. ) ;
#3246 = ORIENTED_EDGE ( 'NONE', *, *, #19914, .F. ) ;
#3247 = CARTESIAN_POINT ( 'NONE',  ( -24.99999999999998934, 45.00100000000031031, 34.99999999999983658 ) ) ;
#3248 = ADVANCED_FACE ( 'NONE', ( #14461 ), #21800, .F. ) ;
#3249 = ORIENTED_EDGE ( 'NONE', *, *, #12437, .F. ) ;
#3250 = EDGE_CURVE ( 'NONE', #20963, #11281, #10779, .T. ) ;
#3251 = CIRCLE ( 'NONE', #22915, 7.500000000000004441 ) ;
#3252 =( BOUNDED_SURFACE ( )  B_SPLINE_SURFACE ( 3, 2, ( 
 ( #6042, #17049, #847 ),
 ( #7982, #2775, #11762 ),
 ( #11882, #6406, #620 ),
 ( #2661, #18955, #21135 ),
 ( #20899, #11651, #390 ),
 ( #13811, #22820, #10059 ),
 ( #9927, #7753, #2418 ),
 ( #9806, #17161, #22702 ) ),
 .UNSPECIFIED., .F., .F., .F. ) 
 B_SPLINE_SURFACE_WITH_KNOTS ( ( 4, 2, 2, 4 ),
 ( 3, 3 ),
 ( 0.03861844051980971304, 0.04325213341840642572, 0.04556897986770477860, 0.04788582631700313841 ),
 ( 0.000000000000000000, 1.000000000000000000 ),
 .UNSPECIFIED. ) 
 GEOMETRIC_REPRESENTATION_ITEM ( )  RATIONAL_B_SPLINE_SURFACE ( (
 ( 1.000000000000000000, 0.8047781759831923454, 1.000000000000000000),
 ( 1.000000000000000000, 0.8123762462805160789, 1.000000000000000000),
 ( 1.000000000000000000, 0.8190659850616602844, 1.000000000000000000),
 ( 1.000000000000000000, 0.8191937571013702124, 1.000000000000000000),
 ( 1.000000000000000000, 0.8176092952780309453, 1.000000000000000000),
 ( 1.000000000000000000, 0.8122962088596628050, 1.000000000000000000),
 ( 1.000000000000000000, 0.8086311330827828936, 1.000000000000000000),
 ( 1.000000000000000000, 0.8047712282214327661, 1.000000000000000000) ) ) 
 REPRESENTATION_ITEM ( '' )  SURFACE ( )  );
#3253 = CARTESIAN_POINT ( 'NONE',  ( 0.000000000000000000, 0.000000000000000000, -9.226681596905677907 ) ) ;
#3254 = DIRECTION ( 'NONE',  ( -0.000000000000000000, 1.000000000000000000, -3.469446951953613794E-15 ) ) ;
#3255 = VECTOR ( 'NONE', #2925, 1000.000000000000000 ) ;
#3256 = ORIENTED_EDGE ( 'NONE', *, *, #18134, .T. ) ;
#3257 = DIRECTION ( 'NONE',  ( -1.000000000000000000, 0.000000000000000000, 0.000000000000000000 ) ) ;
#3258 = CIRCLE ( 'NONE', #9468, 160.0000000000000000 ) ;
#3259 = CIRCLE ( 'NONE', #12952, 45.00000000000000711 ) ;
#3260 = ORIENTED_EDGE ( 'NONE', *, *, #18009, .T. ) ;
#3261 = CARTESIAN_POINT ( 'NONE',  ( 2.500000000000002220, 1.178949249685212086, -2.042000000000002036 ) ) ;
#3262 = ORIENTED_EDGE ( 'NONE', *, *, #22699, .F. ) ;
#3263 = CARTESIAN_POINT ( 'NONE',  ( 0.000000000000000000, -1000.000000000000000, 145.0000119999999697 ) ) ;
#3264 = B_SPLINE_CURVE_WITH_KNOTS ( 'NONE', 3,
 ( #18704, #9437, #15129, #9553, #5453, #16917, #251, #14879 ),
 .UNSPECIFIED., .F., .F.,
 ( 4, 2, 2, 4 ),
 ( 2.465131517071610173E-07, 0.001183067374689837636, 0.001774477805458902699, 0.002365888236227967761 ),
 .UNSPECIFIED. ) ;
#3265 = DIRECTION ( 'NONE',  ( 0.000000000000000000, 0.000000000000000000, -1.000000000000000000 ) ) ;
#3266 = CARTESIAN_POINT ( 'NONE',  ( 0.000000000000000000, -131.9709811566878273, -0.000000000000000000 ) ) ;
#3267 = DIRECTION ( 'NONE',  ( 0.000000000000000000, -0.000000000000000000, 1.000000000000000000 ) ) ;
#3268 = DIRECTION ( 'NONE',  ( 1.000000000000000000, 0.000000000000000000, 0.000000000000000000 ) ) ;
#3269 = ORIENTED_EDGE ( 'NONE', *, *, #21529, .T. ) ;
#3270 = CARTESIAN_POINT ( 'NONE',  ( 20.00000000000000000, 0.000000000000000000, -125.0000000000000000 ) ) ;
#3271 = SHAPE_REPRESENTATION_RELATIONSHIP ( 'NONE' , 'NONE' ,  #4815, #3229 ) ;
#3272 = CIRCLE ( 'NONE', #16782, 45.00000000000000711 ) ;
#3274 = ORIENTED_EDGE ( 'NONE', *, *, #16709, .T. ) ;
#3273 = ORIENTED_EDGE ( 'NONE', *, *, #21507, .T. ) ;
#3275 = DIRECTION ( 'NONE',  ( 1.000000000000000000, 2.832769448823979947E-16, -2.832769448823989808E-16 ) ) ;
#3276 = EDGE_CURVE ( 'NONE', #12504, #22000, #21221, .T. ) ;
#3277 = EDGE_CURVE ( 'NONE', #10884, #4892, #15987, .T. ) ;
#3278 = CARTESIAN_POINT ( 'NONE',  ( -45.00000000000000000, 272.9999999999999432, 5.249999999999973355 ) ) ;
#3279 = CARTESIAN_POINT ( 'NONE',  ( 2.699999999999995737, 0.000000000000000000, -20.30000000000000071 ) ) ;
#3280 = ADVANCED_FACE ( 'NONE', ( #23213 ), #6921, .F. ) ;
#3281 = CYLINDRICAL_SURFACE ( 'NONE', #20382, 45.00000000000000711 ) ;
#3282 = DIRECTION ( 'NONE',  ( 1.000000000000000000, 0.000000000000000000, 0.000000000000000000 ) ) ;
#3283 = AXIS2_PLACEMENT_3D ( 'NONE', #10073, #12028, #13954 ) ;
#3284 = VERTEX_POINT ( 'NONE', #4868 ) ;
#3285 = CARTESIAN_POINT ( 'NONE',  ( 3.750000000000005329, 6.495190528383288253, 0.000000000000000000 ) ) ;
#3286 = ORIENTED_EDGE ( 'NONE', *, *, #6247, .T. ) ;
#3287 = CARTESIAN_POINT ( 'NONE',  ( -128.5330911521627399, -1074.345258785412170, -29.99999999999356604 ) ) ;
#3288 = CARTESIAN_POINT ( 'NONE',  ( 0.000000000000000000, 0.000000000000000000, 169.9999999999999716 ) ) ;
#3289 = CONTEXT_DEPENDENT_SHAPE_REPRESENTATION ( #14642, #12444 ) ;
#3290 = ORIENTED_EDGE ( 'NONE', *, *, #12244, .T. ) ;
#3291 = AXIS2_PLACEMENT_3D ( 'NONE', #1256, #10212, #10333 ) ;
#3292 = EDGE_LOOP ( 'NONE', ( #5402, #8290, #4208, #23445 ) ) ;
#3293 = CARTESIAN_POINT ( 'NONE',  ( 20.55500000000001748, 0.000000000000000000, 0.000000000000000000 ) ) ;
#3294 = DIRECTION ( 'NONE',  ( 1.000000000000000000, 0.000000000000000000, 0.000000000000000000 ) ) ;
#3295 = ORIENTED_EDGE ( 'NONE', *, *, #7592, .F. ) ;
#3296 = LINE ( 'NONE', #1610, #20557 ) ;
#3297 = CARTESIAN_POINT ( 'NONE',  ( 133.9966253006739407, 77.90961723643370362, 28.88679084683407794 ) ) ;
#3298 = CARTESIAN_POINT ( 'NONE',  ( -129.2206655591611764, -1072.408698320350140, -27.94499999999356632 ) ) ;
#3299 = CARTESIAN_POINT ( 'NONE',  ( -79.04925354955163641, -121.5574576620402496, -90.00000000000000000 ) ) ;
#3300 = CARTESIAN_POINT ( 'NONE',  ( -4.211140560182196957, 2.431303136016537803, -3.745885042887433514 ) ) ;
#3301 = AXIS2_PLACEMENT_3D ( 'NONE', #6837, #13774, #21092 ) ;
#3302 = DIRECTION ( 'NONE',  ( 0.000000000000000000, 0.000000000000000000, -1.000000000000000000 ) ) ;
#3303 = EDGE_LOOP ( 'NONE', ( #20738, #7908, #1856 ) ) ;
#3304 = VECTOR ( 'NONE', #13953, 1000.000000000000114 ) ;
#3305 = EDGE_CURVE ( 'NONE', #12407, #18161, #19576, .T. ) ;
#3306 = DIRECTION ( 'NONE',  ( 0.000000000000000000, -1.000000000000000000, 1.287488025362403787E-15 ) ) ;
#3307 = CARTESIAN_POINT ( 'NONE',  ( -2.725741868435985094, 3.045094352034055429, -3.220599429844047012 ) ) ;
#3308 = AXIS2_PLACEMENT_3D ( 'NONE', #10082, #8003, #5835 ) ;
#3309 = EDGE_LOOP ( 'NONE', ( #10169, #7031, #1019, #15364 ) ) ;
#3310 = ADVANCED_FACE ( 'NONE', ( #23331 ), #14321, .F. ) ;
#3311 = DIRECTION ( 'NONE',  ( 0.000000000000000000, -1.000000000000000000, 0.000000000000000000 ) ) ;
#3312 = FACE_OUTER_BOUND ( 'NONE', #4071, .T. ) ;
#3314 = CARTESIAN_POINT ( 'NONE',  ( -285.2300000000000182, 268.4847249064869743, 146.3684637172358691 ) ) ;
#3313 = PRODUCT_DEFINITION_SHAPE ( 'NONE', 'NONE',  #23854 ) ;
#3315 = CONICAL_SURFACE ( 'NONE', #19911, 5.560781378645573980, 1.221730476396046816 ) ;
#3316 = CARTESIAN_POINT ( 'NONE',  ( -158.1195828810602109, 116.4077317428687763, -32.49999999999322853 ) ) ;
#3317 = DIRECTION ( 'NONE',  ( 0.000000000000000000, 0.000000000000000000, -1.000000000000000000 ) ) ;
#3318 = ORIENTED_EDGE ( 'NONE', *, *, #12480, .F. ) ;
#3319 = FACE_BOUND ( 'NONE', #8470, .T. ) ;
#3320 = ORIENTED_EDGE ( 'NONE', *, *, #22824, .T. ) ;
#3321 = CARTESIAN_POINT ( 'NONE',  ( 2.500000000000000000, 0.000000000000000000, 0.000000000000000000 ) ) ;
#3322 = PLANE ( 'NONE',  #18081 ) ;
#3323 = VECTOR ( 'NONE', #5730, 1000.000000000000000 ) ;
#3324 = ORIENTED_EDGE ( 'NONE', *, *, #3934, .T. ) ;
#3325 =( LENGTH_UNIT ( ) NAMED_UNIT ( * ) SI_UNIT ( .MILLI., .METRE. ) );
#3326 = DIRECTION ( 'NONE',  ( 1.000000000000000000, 0.000000000000000000, 0.000000000000000000 ) ) ;
#3327 = DIRECTION ( 'NONE',  ( 1.000000000000000000, 0.000000000000000000, 0.000000000000000000 ) ) ;
#3328 = CARTESIAN_POINT ( 'NONE',  ( 20.55500000000001748, 0.000000000000000000, 0.000000000000000000 ) ) ;
#3329 = CARTESIAN_POINT ( 'NONE',  ( -6.259644161404860030E-16, -4.618802153517027165, -5.000000000000000000 ) ) ;
#3330 = DIRECTION ( 'NONE',  ( 1.000000000000000000, 0.000000000000000000, 0.000000000000000000 ) ) ;
#3331 = ADVANCED_FACE ( 'NONE', ( #6798 ), #8503, .F. ) ;
#3332 = DIRECTION ( 'NONE',  ( 1.000000000000000000, 0.000000000000000000, 0.000000000000000000 ) ) ;
#3333 = ORIENTED_EDGE ( 'NONE', *, *, #19966, .F. ) ;
#3334 = ADVANCED_FACE ( 'NONE', ( #23094 ), #12517, .T. ) ;
#3335 = EDGE_LOOP ( 'NONE', ( #12519, #19471, #19349, #18142 ) ) ;
#3336 = DIRECTION ( 'NONE',  ( 0.000000000000000000, -1.000000000000000000, 0.000000000000000000 ) ) ;
#3337 = AXIS2_PLACEMENT_3D ( 'NONE', #15013, #628, #12988 ) ;
#3338 = DIRECTION ( 'NONE',  ( 0.000000000000000000, -0.4999999999999992784, 0.8660254037844389297 ) ) ;
#3339 = ORIENTED_EDGE ( 'NONE', *, *, #12855, .T. ) ;
#3340 = ORIENTED_EDGE ( 'NONE', *, *, #21968, .F. ) ;
#3341 = DIRECTION ( 'NONE',  ( -1.110223024625155594E-14, 0.000000000000000000, -1.000000000000000000 ) ) ;
#3342 = CARTESIAN_POINT ( 'NONE',  ( 7.112481253774308954, -4.553861071371678726, -7.781689322728511549 ) ) ;
#3343 = ADVANCED_FACE ( 'NONE', ( #3044 ), #8370, .F. ) ;
#3344 = ORIENTED_EDGE ( 'NONE', *, *, #11070, .T. ) ;
#3345 = LINE ( 'NONE', #11462, #16373 ) ;
#3346 = CARTESIAN_POINT ( 'NONE',  ( -3.808014612217195616, 9.322005033491132409, 200.0000120000000550 ) ) ;
#3347 = VERTEX_POINT ( 'NONE', #4994 ) ;
#3348 = DIRECTION ( 'NONE',  ( 0.000000000000000000, 0.000000000000000000, -1.000000000000000000 ) ) ;
#3349 = ADVANCED_FACE ( 'NONE', ( #19830 ), #17327, .T. ) ;
#3350 = VECTOR ( 'NONE', #14502, 1000.000000000000000 ) ;
#3351 = ORIENTED_EDGE ( 'NONE', *, *, #3665, .T. ) ;
#3352 = LINE ( 'NONE', #102, #22254 ) ;
#3353 = CONICAL_SURFACE ( 'NONE', #17252, 4.000000000000000000, 0.8911886515913786111 ) ;
#3354 = DIRECTION ( 'NONE',  ( -8.144298233840332611E-17, 0.000000000000000000, -1.000000000000000000 ) ) ;
#3355 = VERTEX_POINT ( 'NONE', #21401 ) ;
#3356 = ORIENTED_EDGE ( 'NONE', *, *, #12322, .F. ) ;
#3357 = DIRECTION ( 'NONE',  ( -0.000000000000000000, 1.000000000000000000, -3.469446951953613794E-15 ) ) ;
#3358 = DIRECTION ( 'NONE',  ( 1.221966984364620947E-29, 3.495664435217746987E-15, -1.000000000000000000 ) ) ;
#3359 = LINE ( 'NONE', #23763, #3087 ) ;
#3360 = CARTESIAN_POINT ( 'NONE',  ( 0.000000000000000000, 0.000000000000000000, 100.0000000000000000 ) ) ;
#3361 = DIRECTION ( 'NONE',  ( 1.000000000000000000, 0.000000000000000000, 0.000000000000000000 ) ) ;
#3362 = ORIENTED_EDGE ( 'NONE', *, *, #21394, .F. ) ;
#3363 = CYLINDRICAL_SURFACE ( 'NONE', #21096, 2.649999999999971934 ) ;
#3364 = AXIS2_PLACEMENT_3D ( 'NONE', #9388, #12921, #5511 ) ;
#3365 = ADVANCED_FACE ( 'NONE', ( #4743 ), #3281, .T. ) ;
#3366 = EDGE_CURVE ( 'NONE', #9294, #6807, #18457, .T. ) ;
#3367 = AXIS2_PLACEMENT_3D ( 'NONE', #11000, #18321, #14464 ) ;
#3368 = CARTESIAN_POINT ( 'NONE',  ( -287.4000000000014552, -127.0000000000000568, -146.4928932188134070 ) ) ;
#3369 = AXIS2_PLACEMENT_3D ( 'NONE', #12581, #1548, #8933 ) ;
#3370 = CARTESIAN_POINT ( 'NONE',  ( 85.22886158240964960, -117.3074641843666370, -90.00000000000000000 ) ) ;
#3371 = EDGE_LOOP ( 'NONE', ( #19340, #19857, #830, #21633 ) ) ;
#3372 = CARTESIAN_POINT ( 'NONE',  ( -0.2791032213812780771, 8.821394357840562250, -7.929128246061909024 ) ) ;
#3373 = EDGE_CURVE ( 'NONE', #6031, #14121, #4598, .T. ) ;
#3374 = ADVANCED_FACE ( 'NONE', ( #12272 ), #10198, .F. ) ;
#3375 = VERTEX_POINT ( 'NONE', #13973 ) ;
#3376 = DIRECTION ( 'NONE',  ( -1.000000000000000000, -0.000000000000000000, -0.000000000000000000 ) ) ;
#3377 = CONICAL_SURFACE ( 'NONE', #15356, 2.055000000000001492, 0.7853981633974633780 ) ;
#3378 = VERTEX_POINT ( 'NONE', #12156 ) ;
#3379 = DIRECTION ( 'NONE',  ( 0.000000000000000000, -4.183096374613631247E-18, 1.000000000000000000 ) ) ;
#3380 = VECTOR ( 'NONE', #3868, 1000.000000000000000 ) ;
#3381 = CIRCLE ( 'NONE', #14239, 2.041999999999999815 ) ;
#3382 = AXIS2_PLACEMENT_3D ( 'NONE', #13638, #9741, #894 ) ;
#3383 = CYLINDRICAL_SURFACE ( 'NONE', #13473, 2.649999999999971934 ) ;
#3384 = CARTESIAN_POINT ( 'NONE',  ( 125.6576742947584364, -1090.747768901066138, -28.46728581292316562 ) ) ;
#3385 = AXIS2_PLACEMENT_3D ( 'NONE', #22286, #16863, #17233 ) ;
#3386 = CARTESIAN_POINT ( 'NONE',  ( -7.500000000000000888, -3.640541674360520119, -0.7158139487964623182 ) ) ;
#3387 = ORIENTED_EDGE ( 'NONE', *, *, #10710, .F. ) ;
#3388 = CYLINDRICAL_SURFACE ( 'NONE', #8399, 2.649999999999971934 ) ;
#3389 =( NAMED_UNIT ( * ) SI_UNIT ( $, .STERADIAN. ) SOLID_ANGLE_UNIT ( ) );
#3391 = EDGE_LOOP ( 'NONE', ( #6494, #9496, #6292, #22641 ) ) ;
#3390 = ORIENTED_EDGE ( 'NONE', *, *, #3857, .T. ) ;
#3392 = CARTESIAN_POINT ( 'NONE',  ( 45.00000000000004263, -47.79999999999967031, 250.0000000000002274 ) ) ;
#3393 = DIRECTION ( 'NONE',  ( 0.000000000000000000, -0.000000000000000000, 1.000000000000000000 ) ) ;
#3394 = CARTESIAN_POINT ( 'NONE',  ( -79.99999999999995737, -62.00000000000001421, 5.199999999999997513 ) ) ;
#3395 = ORIENTED_EDGE ( 'NONE', *, *, #22954, .T. ) ;
#3396 = CIRCLE ( 'NONE', #18817, 2.199999999999979750 ) ;
#3397 = DIRECTION ( 'NONE',  ( 0.000000000000000000, -1.000000000000000000, 0.000000000000000000 ) ) ;
#3398 = ADVANCED_FACE ( 'NONE', ( #12553, #19868 ), #21220, .F. ) ;
#3399 = AXIS2_PLACEMENT_3D ( 'NONE', #22275, #199, #18195 ) ;
#3400 = EDGE_CURVE ( 'NONE', #907, #20119, #13897, .T. ) ;
#3401 = VECTOR ( 'NONE', #9352, 1000.000000000000000 ) ;
#3402 = LINE ( 'NONE', #18155, #676 ) ;
#3403 = VECTOR ( 'NONE', #8849, 1000.000000000000000 ) ;
#3404 = EDGE_CURVE ( 'NONE', #19823, #9902, #4907, .T. ) ;
#3405 = ORIENTED_EDGE ( 'NONE', *, *, #21627, .T. ) ;
#3406 = ADVANCED_FACE ( 'NONE', ( #5141 ), #2842, .F. ) ;
#3407 = CARTESIAN_POINT ( 'NONE',  ( 0.000000000000000000, 0.000000000000000000, -90.00000000000000000 ) ) ;
#3408 = FACE_OUTER_BOUND ( 'NONE', #7905, .T. ) ;
#3409 = AXIS2_PLACEMENT_3D ( 'NONE', #4191, #340, #11608 ) ;
#3410 = CONTEXT_DEPENDENT_SHAPE_REPRESENTATION ( #17291, #15485 ) ;
#3411 = EDGE_LOOP ( 'NONE', ( #1802, #8813 ) ) ;
#3412 = EDGE_LOOP ( 'NONE', ( #21473, #3196 ) ) ;
#3413 = EDGE_CURVE ( 'NONE', #4308, #21081, #13121, .T. ) ;
#3414 = CARTESIAN_POINT ( 'NONE',  ( 125.6576742947588485, -1090.747768901065228, 31.53271418707689122 ) ) ;
#3415 = VERTEX_POINT ( 'NONE', #23246 ) ;
#3416 = ADVANCED_FACE ( 'NONE', ( #19381 ), #6719, .F. ) ;
#3417 = CARTESIAN_POINT ( 'NONE',  ( -282.2000000000012960, -74.99999999999899103, 90.00000000000000000 ) ) ;
#3418 = CARTESIAN_POINT ( 'NONE',  ( 134.1180124237192501, 77.70044921554838879, 30.32918505548582289 ) ) ;
#3419 = DIRECTION ( 'NONE',  ( -1.000000000000000000, 0.000000000000000000, 0.000000000000000000 ) ) ;
#3420 = PRODUCT_DEFINITION_SHAPE ( 'NONE', 'NONE',  #9630 ) ;
#3421 = VECTOR ( 'NONE', #4763, 1000.000000000000000 ) ;
#3422 = DIRECTION ( 'NONE',  ( 1.000000000000000000, 0.000000000000000000, 0.000000000000000000 ) ) ;
#3424 = VECTOR ( 'NONE', #14180, 1000.000000000000114 ) ;
#3423 =( GEOMETRIC_REPRESENTATION_CONTEXT ( 3 ) GLOBAL_UNCERTAINTY_ASSIGNED_CONTEXT ( ( #20728 ) ) GLOBAL_UNIT_ASSIGNED_CONTEXT ( ( #18486, #22097, #20411 ) ) REPRESENTATION_CONTEXT ( 'NONE', 'WORKASPACE' ) );
#3425 = DIRECTION ( 'NONE',  ( 1.000000000000000000, 0.000000000000000000, 0.000000000000000000 ) ) ;
#3426 = CARTESIAN_POINT ( 'NONE',  ( -155.0000000000000284, -494.4690652294806341, 30.00000000000648015 ) ) ;
#3427 = VECTOR ( 'NONE', #7829, 1000.000000000000000 ) ;
#3428 = AXIS2_PLACEMENT_3D ( 'NONE', #9803, #845, #11760 ) ;
#3429 = ORIENTED_EDGE ( 'NONE', *, *, #21555, .F. ) ;
#3430 = DIRECTION ( 'NONE',  ( 0.000000000000000000, 0.000000000000000000, -1.000000000000000000 ) ) ;
#3431 = DIRECTION ( 'NONE',  ( -1.000000000000000000, -0.000000000000000000, -0.000000000000000000 ) ) ;
#3432 = ORIENTED_EDGE ( 'NONE', *, *, #12453, .T. ) ;
#3433 = DIRECTION ( 'NONE',  ( 0.000000000000000000, -1.000000000000000000, 0.000000000000000000 ) ) ;
#3434 = EDGE_CURVE ( 'NONE', #15247, #20600, #1504, .T. ) ;
#3435 = CARTESIAN_POINT ( 'NONE',  ( 155.0000000000000284, -500.0000000000000000, -29.99999999999997158 ) ) ;
#3436 = CARTESIAN_POINT ( 'NONE',  ( -281.3333820183296439, 269.5350371479512432, 145.6220388411722695 ) ) ;
#3437=STYLED_ITEM('',(#23920),#20279);
#3438 = VECTOR ( 'NONE', #13932, 1000.000000000000000 ) ;
#3439 = CARTESIAN_POINT ( 'NONE',  ( -44.99999999999995026, -59.79999999999969162, 102.3500000000002359 ) ) ;
#3440 = CIRCLE ( 'NONE', #20030, 2.499999999999998668 ) ;
#3441 = CARTESIAN_POINT ( 'NONE',  ( 281.3683070494394087, 268.4816199723481986, -150.1663417894421571 ) ) ;
#3442 = VECTOR ( 'NONE', #13251, 1000.000000000000000 ) ;
#3443 = VECTOR ( 'NONE', #13694, 1000.000000000000000 ) ;
#3444 = VERTEX_POINT ( 'NONE', #19503 ) ;
#3445 = VECTOR ( 'NONE', #1737, 1000.000000000000000 ) ;
#3446 = VECTOR ( 'NONE', #13913, 1000.000000000000000 ) ;
#3447 = CARTESIAN_POINT ( 'NONE',  ( 146.0000000000002274, -210.0000000000003411, -29.99999999999356604 ) ) ;
#3448 = ORIENTED_EDGE ( 'NONE', *, *, #14467, .T. ) ;
#3449 = DIRECTION ( 'NONE',  ( 0.000000000000000000, 0.000000000000000000, -1.000000000000000000 ) ) ;
#3450 = B_SPLINE_CURVE_WITH_KNOTS ( 'NONE', 3,
 ( #7520, #14912, #5127, #61, #1496, #3300 ),
 .UNSPECIFIED., .F., .F.,
 ( 4, 2, 4 ),
 ( 0.002452478801916376308, 0.003676905084148007850, 0.004901331366379639391 ),
 .UNSPECIFIED. ) ;
#3451 = FACE_OUTER_BOUND ( 'NONE', #5420, .T. ) ;
#3452 = EDGE_CURVE ( 'NONE', #14004, #21515, #19234, .T. ) ;
#3453 = EDGE_CURVE ( 'NONE', #21308, #9451, #23500, .T. ) ;
#3454 = DIRECTION ( 'NONE',  ( -3.495664435217746987E-15, 1.000000000000000000, 0.000000000000000000 ) ) ;
#3455 = ORIENTED_EDGE ( 'NONE', *, *, #23144, .F. ) ;
#3456 = DIRECTION ( 'NONE',  ( 0.000000000000000000, 0.000000000000000000, -1.000000000000000000 ) ) ;
#3457 = LINE ( 'NONE', #19877, #13912 ) ;
#3458 = CARTESIAN_POINT ( 'NONE',  ( 282.2000000000013529, -127.0000000000000568, -146.4928932188134070 ) ) ;
#3459 = CARTESIAN_POINT ( 'NONE',  ( -281.4928932188135491, -132.2000000000000455, 152.4000000000014268 ) ) ;
#3460 = FACE_OUTER_BOUND ( 'NONE', #12390, .T. ) ;
#3461 = CARTESIAN_POINT ( 'NONE',  ( -12.52876685377504451, 21.69578997558840072, 145.0000119999999697 ) ) ;
#3462 = ORIENTED_EDGE ( 'NONE', *, *, #14840, .T. ) ;
#3463 = ORIENTED_EDGE ( 'NONE', *, *, #2648, .T. ) ;
#3465 = CIRCLE ( 'NONE', #5380, 2.499999999999998668 ) ;
#3464 = AXIS2_PLACEMENT_3D ( 'NONE', #23447, #12629, #19708 ) ;
#3466 = CYLINDRICAL_SURFACE ( 'NONE', #1440, 2.500000000000002220 ) ;
#3467 = DIRECTION ( 'NONE',  ( 0.000000000000000000, 0.000000000000000000, 1.000000000000000000 ) ) ;
#3468 = AXIS2_PLACEMENT_3D ( 'NONE', #2334, #22383, #20560 ) ;
#3469 = ORIENTED_EDGE ( 'NONE', *, *, #22005, .T. ) ;
#3470 = AXIS2_PLACEMENT_3D ( 'NONE', #2408, #6034, #11754 ) ;
#3471 = CARTESIAN_POINT ( 'NONE',  ( 0.000000000000000000, 0.000000000000000000, -100.0000000000000000 ) ) ;
#3472 = CARTESIAN_POINT ( 'NONE',  ( 3.000000000000002665, 3.043247295881173007E-15, 24.69999999999999929 ) ) ;
#3473 = ORIENTED_EDGE ( 'NONE', *, *, #11258, .T. ) ;
#3474 = CARTESIAN_POINT ( 'NONE',  ( 280.8708543776410806, 269.1520027839447948, 146.7592670532760053 ) ) ;
#3475 = VECTOR ( 'NONE', #2914, 1000.000000000000000 ) ;
#3476 = DIRECTION ( 'NONE',  ( 0.000000000000000000, 0.000000000000000000, -1.000000000000000000 ) ) ;
#3477 = ORIENTED_EDGE ( 'NONE', *, *, #21259, .T. ) ;
#3478 = PLANE ( 'NONE',  #21787 ) ;
#3479 = ORIENTED_EDGE ( 'NONE', *, *, #2101, .T. ) ;
#3480 = CARTESIAN_POINT ( 'NONE',  ( -45.24999999999994316, 100.0000000000000000, 150.2000000000009550 ) ) ;
#3481 = CARTESIAN_POINT ( 'NONE',  ( -136.1785371930672000, -1074.029921987505077, 32.37408494914631518 ) ) ;
#3482 = AXIS2_PLACEMENT_3D ( 'NONE', #12755, #10924, #9088 ) ;
#3484 = VECTOR ( 'NONE', #7444, 1000.000000000000000 ) ;
#3483 = CARTESIAN_POINT ( 'NONE',  ( -85.22886158240879695, 117.3074641843673049, -90.00000000000000000 ) ) ;
#3485 = VERTEX_POINT ( 'NONE', #2953 ) ;
#3486 = ORIENTED_EDGE ( 'NONE', *, *, #2725, .T. ) ;
#3487 = CARTESIAN_POINT ( 'NONE',  ( -31.74999999999995737, 0.000000000000000000, 0.000000000000000000 ) ) ;
#3488 = CIRCLE ( 'NONE', #20829, 2.500000000000000888 ) ;
#3489 = AXIS2_PLACEMENT_3D ( 'NONE', #13729, #22848, #11795 ) ;
#3490 = DIRECTION ( 'NONE',  ( -1.000000000000000000, -0.000000000000000000, -0.000000000000000000 ) ) ;
#3491 = LINE ( 'NONE', #9058, #4168 ) ;
#3492 = CARTESIAN_POINT ( 'NONE',  ( 3.333333333333332593, 2.694301256218250007, -3.300726591567078483 ) ) ;
#3493 = ORIENTED_EDGE ( 'NONE', *, *, #2966, .F. ) ;
#3494 = CARTESIAN_POINT ( 'NONE',  ( -22.47082401081931735, -11.07878015919985515, 145.0000119999999697 ) ) ;
#3495 = SURFACE_STYLE_USAGE ( .BOTH. , #5756 ) ;
#3496 = DIRECTION ( 'NONE',  ( -1.350636282998972974E-14, 0.000000000000000000, -1.000000000000000000 ) ) ;
#3497 = DIRECTION ( 'NONE',  ( 1.000000000000000000, 0.000000000000000000, 0.000000000000000000 ) ) ;
#3498 = EDGE_LOOP ( 'NONE', ( #22994, #15294, #1580, #15933 ) ) ;
#3499 = DIRECTION ( 'NONE',  ( -6.753181414994864868E-15, 6.753181414994864868E-15, -1.000000000000000000 ) ) ;
#3500 = ORIENTED_EDGE ( 'NONE', *, *, #19418, .T. ) ;
#3501 = CARTESIAN_POINT ( 'NONE',  ( 2.500000000000000000, 0.000000000000000000, 0.000000000000000000 ) ) ;
#3502 = ORIENTED_EDGE ( 'NONE', *, *, #15244, .T. ) ;
#3503 = ADVANCED_FACE ( 'NONE', ( #3091 ), #9228, .F. ) ;
#3504 = DIRECTION ( 'NONE',  ( -0.000000000000000000, -0.000000000000000000, -1.000000000000000000 ) ) ;
#3505 = FILL_AREA_STYLE ('',( #14876 ) ) ;
#3506 = ADVANCED_FACE ( 'NONE', ( #1027 ), #4976, .T. ) ;
#3507 = EDGE_CURVE ( 'NONE', #13434, #18427, #730, .T. ) ;
#3508 = FACE_OUTER_BOUND ( 'NONE', #3669, .T. ) ;
#3509 =( REPRESENTATION_RELATIONSHIP ('NONE','NONE', #10127, #18083 ) REPRESENTATION_RELATIONSHIP_WITH_TRANSFORMATION ( #18709 )SHAPE_REPRESENTATION_RELATIONSHIP( ) );
#3510 = LINE ( 'NONE', #9435, #20511 ) ;
#3511 = FACE_OUTER_BOUND ( 'NONE', #8305, .T. ) ;
#3512 = VERTEX_POINT ( 'NONE', #14002 ) ;
#3513 = DIRECTION ( 'NONE',  ( 0.7071067811865320296, 8.659560562355062281E-17, 0.7071067811865631159 ) ) ;
#3514 = SURFACE_STYLE_FILL_AREA ( #16686 ) ;
#3515 = EDGE_CURVE ( 'NONE', #10685, #3355, #11779, .T. ) ;
#3517 = ORIENTED_EDGE ( 'NONE', *, *, #16077, .T. ) ;
#3516 = ORIENTED_EDGE ( 'NONE', *, *, #21211, .T. ) ;
#3518 = DIRECTION ( 'NONE',  ( 0.000000000000000000, 0.000000000000000000, 1.000000000000000000 ) ) ;
#3519 = DIRECTION ( 'NONE',  ( -0.000000000000000000, -0.000000000000000000, 1.000000000000000000 ) ) ;
#3520 = CARTESIAN_POINT ( 'NONE',  ( -129.2206655591611764, -1072.408698320350140, -29.99999999999356604 ) ) ;
#3521 = VERTEX_POINT ( 'NONE', #12803 ) ;
#3522 = DIRECTION ( 'NONE',  ( -0.000000000000000000, -0.000000000000000000, 1.000000000000000000 ) ) ;
#3523 = DIRECTION ( 'NONE',  ( 5.478074134663600261E-16, -1.000000000000000000, 0.000000000000000000 ) ) ;
#3524 = ORIENTED_EDGE ( 'NONE', *, *, #13067, .F. ) ;
#3525 = PLANE ( 'NONE',  #22326 ) ;
#3526 = DIRECTION ( 'NONE',  ( 0.000000000000000000, 0.000000000000000000, -1.000000000000000000 ) ) ;
#3527 = EDGE_LOOP ( 'NONE', ( #3784, #22324, #12867 ) ) ;
#3528 = ORIENTED_EDGE ( 'NONE', *, *, #4495, .F. ) ;
#3529 = DIRECTION ( 'NONE',  ( 3.736327486719275871E-16, -1.000000000000000000, 3.469446951953613794E-15 ) ) ;
#3530 = ORIENTED_EDGE ( 'NONE', *, *, #11258, .F. ) ;
#3531 = CARTESIAN_POINT ( 'NONE',  ( -128.2695163047658298, 87.01699568756195902, 32.42126403526987843 ) ) ;
#3532 = DIRECTION ( 'NONE',  ( 0.000000000000000000, 0.000000000000000000, 1.000000000000000000 ) ) ;
#3533 = CARTESIAN_POINT ( 'NONE',  ( -34.75000000000005684, 100.0000000000000000, 150.2000000000009550 ) ) ;
#3534 = EDGE_CURVE ( 'NONE', #19310, #15178, #14926, .T. ) ;
#3535 = CARTESIAN_POINT ( 'NONE',  ( 72.64999999999999147, -87.33333333333332860, 3.000000000000000000 ) ) ;
#3536 = CARTESIAN_POINT ( 'NONE',  ( 281.4928932188133217, -127.0000000000000568, 152.4000000000014268 ) ) ;
#3537 = SURFACE_STYLE_USAGE ( .BOTH. , #16715 ) ;
#3538 = EDGE_CURVE ( 'NONE', #12643, #17916, #11599, .T. ) ;
#3539 = EDGE_CURVE ( 'NONE', #15114, #5008, #4223, .T. ) ;
#3540 = ORIENTED_EDGE ( 'NONE', *, *, #19795, .T. ) ;
#3541 = CARTESIAN_POINT ( 'NONE',  ( 0.000000000000000000, 0.000000000000000000, 0.000000000000000000 ) ) ;
#3542 = CARTESIAN_POINT ( 'NONE',  ( -7.500000000000000888, 3.988838049906426875, -0.8529248949437632232 ) ) ;
#3543 = CARTESIAN_POINT ( 'NONE',  ( 0.000000000000000000, 0.000000000000000000, -90.00000000000000000 ) ) ;
#3544 = EDGE_LOOP ( 'NONE', ( #13861, #9400, #11674, #16688, #16061 ) ) ;
#3545 = EDGE_CURVE ( 'NONE', #7634, #10526, #9256, .T. ) ;
#3546 = CARTESIAN_POINT ( 'NONE',  ( 280.3113419039144105, 269.8873946496627809, -145.7095819834011650 ) ) ;
#3547 = LINE ( 'NONE', #18279, #18346 ) ;
#3548 = VECTOR ( 'NONE', #22573, 1000.000000000000000 ) ;
#3549 = CARTESIAN_POINT ( 'NONE',  ( -281.3610889986683219, 272.8646579186752774, 145.2488155364689248 ) ) ;
#3550 = LINE ( 'NONE', #3316, #12703 ) ;
#3551 = CARTESIAN_POINT ( 'NONE',  ( -79.04925354955163641, -121.5574576620402496, -2.775557561562891351E-14 ) ) ;
#3552 = ORIENTED_EDGE ( 'NONE', *, *, #17868, .F. ) ;
#3553 = LINE ( 'NONE', #18530, #2092 ) ;
#3554 = VERTEX_POINT ( 'NONE', #11209 ) ;
#3555 = CARTESIAN_POINT ( 'NONE',  ( 0.6666666666666658525, -4.233901974057276085, -3.300726591567086476 ) ) ;
#3556 = CARTESIAN_POINT ( 'NONE',  ( -281.4928932188135491, -127.0000000000000568, 147.2000000000013813 ) ) ;
#3557 = ORIENTED_EDGE ( 'NONE', *, *, #19053, .T. ) ;
#3558 = CARTESIAN_POINT ( 'NONE',  ( -3.750000000000004885, 6.495190528383289141, 0.000000000000000000 ) ) ;
#3559 = CARTESIAN_POINT ( 'NONE',  ( 124.2735041650576449, -1092.634345841123832, -32.48402282453940160 ) ) ;
#3560 = DIRECTION ( 'NONE',  ( -1.000000000000000000, 0.000000000000000000, 0.000000000000000000 ) ) ;
#3561 = DIRECTION ( 'NONE',  ( -0.000000000000000000, -0.000000000000000000, 1.000000000000000000 ) ) ;
#3562 = FACE_BOUND ( 'NONE', #2065, .T. ) ;
#3563 = CARTESIAN_POINT ( 'NONE',  ( -37.68333333333334423, -89.99999999999997158, 3.000000000000001332 ) ) ;
#3564 = CARTESIAN_POINT ( 'NONE',  ( -22.47082401081932090, 11.07878015919984804, 145.0000119999999697 ) ) ;
#3565 = EDGE_LOOP ( 'NONE', ( #5410, #19936, #9737, #16180 ) ) ;
#3566 = ORIENTED_EDGE ( 'NONE', *, *, #20563, .F. ) ;
#3567 = DIRECTION ( 'NONE',  ( 1.000000000000000000, -0.000000000000000000, 6.982962677686266711E-15 ) ) ;
#3568 = DIRECTION ( 'NONE',  ( -0.000000000000000000, 0.8660254037844390407, 0.4999999999999993339 ) ) ;
#3569 = ORIENTED_EDGE ( 'NONE', *, *, #16613, .T. ) ;
#3570 = CARTESIAN_POINT ( 'NONE',  ( -56.99999999999995737, -62.00000000000001421, -3.122502256758252770E-14 ) ) ;
#3571 = DIRECTION ( 'NONE',  ( -1.110223024625155594E-14, 0.000000000000000000, -1.000000000000000000 ) ) ;
#3572 = EDGE_CURVE ( 'NONE', #15996, #6254, #22032, .T. ) ;
#3573 = EDGE_CURVE ( 'NONE', #5614, #14374, #15040, .T. ) ;
#3574 = EDGE_CURVE ( 'NONE', #8832, #13580, #22258, .T. ) ;
#3575 = ORIENTED_EDGE ( 'NONE', *, *, #7698, .T. ) ;
#3576 = DIRECTION ( 'NONE',  ( 0.000000000000000000, 0.000000000000000000, 1.000000000000000000 ) ) ;
#3577 = CARTESIAN_POINT ( 'NONE',  ( -69.99999999999997158, -87.33333333333338544, 0.000000000000000000 ) ) ;
#3578 = EDGE_LOOP ( 'NONE', ( #16303, #3575, #14895, #19374 ) ) ;
#3579 = CARTESIAN_POINT ( 'NONE',  ( 153.5653415408401941, -1122.352966361446079, -29.99999999999322498 ) ) ;
#3580 = B_SPLINE_CURVE_WITH_KNOTS ( 'NONE', 3,
 ( #19295, #2758, #8433, #21241, #23395, #4693 ),
 .UNSPECIFIED., .F., .F.,
 ( 4, 2, 4 ),
 ( 0.000000000000000000, 0.0004189869898914152461, 0.0008379739797828304922 ),
 .UNSPECIFIED. ) ;
#3581 = CARTESIAN_POINT ( 'NONE',  ( 7.263825692932297962, 4.945657111639574666, -7.907570769506046204 ) ) ;
#3582 = AXIS2_PLACEMENT_3D ( 'NONE', #13644, #4890, #19370 ) ;
#3583 = ORIENTED_EDGE ( 'NONE', *, *, #21673, .F. ) ;
#3584 = CARTESIAN_POINT ( 'NONE',  ( 0.000000000000000000, 0.000000000000000000, 4.000000000000000000 ) ) ;
#3585 = DIRECTION ( 'NONE',  ( -1.000000000000000000, 3.495664435217746987E-15, 0.000000000000000000 ) ) ;
#3586 = CARTESIAN_POINT ( 'NONE',  ( -4.101948962585906244, 2.368261337751074169, -3.681124513963621503 ) ) ;
#3587 = ORIENTED_EDGE ( 'NONE', *, *, #6215, .T. ) ;
#3588 = ORIENTED_EDGE ( 'NONE', *, *, #21314, .T. ) ;
#3589 = DIRECTION ( 'NONE',  ( -0.000000000000000000, 1.000000000000000000, -3.469446951953613794E-15 ) ) ;
#3590 = PLANE ( 'NONE',  #9679 ) ;
#3591 = CARTESIAN_POINT ( 'NONE',  ( -6.439685834476978954, 4.942299687812971243, -7.659344964963200830 ) ) ;
#3592 = CARTESIAN_POINT ( 'NONE',  ( 65.00000000000004263, -52.79999999999959925, 65.00000000000018474 ) ) ;
#3593 = AXIS2_PLACEMENT_3D ( 'NONE', #4819, #9914, #19182 ) ;
#3594 = VECTOR ( 'NONE', #20916, 1000.000000000000000 ) ;
#3595 = VERTEX_POINT ( 'NONE', #18527 ) ;
#3596 = CARTESIAN_POINT ( 'NONE',  ( 281.4928932188133786, 5.173457871231061435E-13, 150.2000000000009550 ) ) ;
#3597 = UNCERTAINTY_MEASURE_WITH_UNIT (LENGTH_MEASURE( 1.000000000000000082E-05 ), #16013, 'distance_accuracy_value', 'NONE');
#3598 = DIRECTION ( 'NONE',  ( 0.000000000000000000, -3.495664435217746987E-15, 1.000000000000000000 ) ) ;
#3599 = LINE ( 'NONE', #6774, #2930 ) ;
#3600 = ORIENTED_EDGE ( 'NONE', *, *, #16411, .T. ) ;
#3601 = CARTESIAN_POINT ( 'NONE',  ( -2.352990130084580066E-16, 8.660254037844390851, -7.564335161054497547 ) ) ;
#3602 =( GEOMETRIC_REPRESENTATION_CONTEXT ( 3 ) GLOBAL_UNCERTAINTY_ASSIGNED_CONTEXT ( ( #22799 ) ) GLOBAL_UNIT_ASSIGNED_CONTEXT ( ( #6970, #12561, #8917 ) ) REPRESENTATION_CONTEXT ( 'NONE', 'WORKASPACE' ) );
#3603 = ORIENTED_EDGE ( 'NONE', *, *, #7494, .T. ) ;
#3604 = PRODUCT ( 'belt', 'belt', '', ( #3834 ) ) ;
#3605 = VECTOR ( 'NONE', #9548, 1000.000000000000000 ) ;
#3606 = PLANE ( 'NONE',  #8296 ) ;
#3607 = CARTESIAN_POINT ( 'NONE',  ( -1.274258131565027874, -3.883108878240886241, -3.220599429844051009 ) ) ;
#3608 = VERTEX_POINT ( 'NONE', #5611 ) ;
#3609 = DIRECTION ( 'NONE',  ( 0.000000000000000000, -1.000000000000000000, -0.000000000000000000 ) ) ;
#3610 = PLANE ( 'NONE',  #7244 ) ;
#3611 = DIRECTION ( 'NONE',  ( 0.3090169943749441761, 0.9510565162951546414, 0.000000000000000000 ) ) ;
#3612 = CARTESIAN_POINT ( 'NONE',  ( 0.000000000000000000, 1.865214261513747767E-15, 138.9999999999999716 ) ) ;
#3613 = VERTEX_POINT ( 'NONE', #3908 ) ;
#3614 = CYLINDRICAL_SURFACE ( 'NONE', #20322, 2.500000000000002220 ) ;
#3615 = DIRECTION ( 'NONE',  ( 0.000000000000000000, 0.000000000000000000, -1.000000000000000000 ) ) ;
#3616 = SHAPE_REPRESENTATION_RELATIONSHIP ( 'NONE' , 'NONE' ,  #18083, #7558 ) ;
#3617 = EDGE_CURVE ( 'NONE', #12251, #16080, #14698, .T. ) ;
#3618 = AXIS2_PLACEMENT_3D ( 'NONE', #18402, #1861, #1987 ) ;
#3620 = ORIENTED_EDGE ( 'NONE', *, *, #21014, .T. ) ;
#3619 = ORIENTED_EDGE ( 'NONE', *, *, #4415, .T. ) ;
#3621 = CARTESIAN_POINT ( 'NONE',  ( -70.00000000000000000, -112.6666666666666998, 119.9999999999999716 ) ) ;
#3622 = CARTESIAN_POINT ( 'NONE',  ( 99.99999999999987210, -127.0000000000000568, 152.4000000000014268 ) ) ;
#3623 = DIRECTION ( 'NONE',  ( -0.7232617928448825673, 0.6905739489807055653, 6.982962677686266711E-15 ) ) ;
#3624 = ORIENTED_EDGE ( 'NONE', *, *, #149, .T. ) ;
#3625 = AXIS2_PLACEMENT_3D ( 'NONE', #22941, #2427, #20207 ) ;
#3626 = EDGE_CURVE ( 'NONE', #6769, #17922, #17733, .T. ) ;
#3627 = CYLINDRICAL_SURFACE ( 'NONE', #12248, 5.249999999999942268 ) ;
#3628 = ADVANCED_FACE ( 'NONE', ( #5731 ), #11077, .T. ) ;
#3629 = LINE ( 'NONE', #1477, #13456 ) ;
#3630 = VERTEX_POINT ( 'NONE', #72 ) ;
#3631 = LINE ( 'NONE', #16455, #1511 ) ;
#3632 = CARTESIAN_POINT ( 'NONE',  ( 312.2000000000013529, -129.2000000000000455, 146.4928932188134638 ) ) ;
#3633 = EDGE_CURVE ( 'NONE', #13320, #22438, #298, .T. ) ;
#3634 = CONTEXT_DEPENDENT_SHAPE_REPRESENTATION ( #19743, #11836 ) ;
#3635 = ORIENTED_EDGE ( 'NONE', *, *, #3677, .F. ) ;
#3636 = APPLICATION_CONTEXT ( 'automotive_design' ) ;
#3637 = AXIS2_PLACEMENT_3D ( 'NONE', #21825, #10886, #18102 ) ;
#3638 = ORIENTED_EDGE ( 'NONE', *, *, #20535, .T. ) ;
#3639 = LINE ( 'NONE', #14904, #13374 ) ;
#3640 = ORIENTED_EDGE ( 'NONE', *, *, #8742, .F. ) ;
#3641 = CARTESIAN_POINT ( 'NONE',  ( 12.52393590769071174, -978.3010413347997201, -145.0000000000001421 ) ) ;
#3642 = CARTESIAN_POINT ( 'NONE',  ( 133.8100684787063983, 78.22965734068104382, 28.34183984639741283 ) ) ;
#3643 = CARTESIAN_POINT ( 'NONE',  ( 4.000000000000000888, -0.8578082829538523635, -3.433262215449808696 ) ) ;
#3644 = CLOSED_SHELL ( 'NONE', ( #5809, #5776, #21372, #12600, #135, #6832, #17905, #20973, #15146, #16611, #17623, #16392, #12431, #11501, #3398, #22865, #18846, #17040, #19591, #4140, #2977, #1039, #20660, #8312, #15858, #7874, #9616, #22930, #1175, #22832, #22592, #9292 ) ) ;
#3645 = DIRECTION ( 'NONE',  ( -0.000000000000000000, -0.000000000000000000, 1.000000000000000000 ) ) ;
#3646 = DIRECTION ( 'NONE',  ( 0.000000000000000000, -1.000000000000000000, 0.000000000000000000 ) ) ;
#3647 = LINE ( 'NONE', #7521, #3442 ) ;
#3648 = ORIENTED_EDGE ( 'NONE', *, *, #9452, .T. ) ;
#3649 = DIRECTION ( 'NONE',  ( 0.000000000000000000, 0.000000000000000000, 1.000000000000000000 ) ) ;
#3650 = DIRECTION ( 'NONE',  ( 1.000000000000000000, 0.000000000000000000, 0.000000000000000000 ) ) ;
#3651 = CIRCLE ( 'NONE', #18698, 24.99999999999998224 ) ;
#3652 = CARTESIAN_POINT ( 'NONE',  ( -4.141042297810615835, 2.227970268150415656, -3.687027686973619822 ) ) ;
#3653 = ORIENTED_EDGE ( 'NONE', *, *, #4860, .T. ) ;
#3654 = LINE ( 'NONE', #5376, #15818 ) ;
#3655 = EDGE_CURVE ( 'NONE', #22159, #6854, #18918, .T. ) ;
#3656 = DIRECTION ( 'NONE',  ( 0.000000000000000000, -1.000000000000000000, 0.000000000000000000 ) ) ;
#3657 = CARTESIAN_POINT ( 'NONE',  ( 7.499999999999999112, 0.3744244963005059490, 1.526918059583750369E-15 ) ) ;
#3658 = AXIS2_PLACEMENT_3D ( 'NONE', #18692, #243, #5808 ) ;
#3659 = AXIS2_PLACEMENT_3D ( 'NONE', #12726, #21737, #5197 ) ;
#3660 = DIRECTION ( 'NONE',  ( -0.000000000000000000, 1.000000000000000000, -0.000000000000000000 ) ) ;
#3661 = CARTESIAN_POINT ( 'NONE',  ( -122.8605704798723082, 82.74225173005861222, 30.00000000000641620 ) ) ;
#3662 = EDGE_CURVE ( 'NONE', #14636, #13229, #1142, .T. ) ;
#3663 = EDGE_LOOP ( 'NONE', ( #16770, #8204 ) ) ;
#3664 = CARTESIAN_POINT ( 'NONE',  ( -44.99999999999995026, -52.79999999999967741, 105.0000000000001990 ) ) ;
#3665 = EDGE_CURVE ( 'NONE', #13236, #2021, #20937, .T. ) ;
#3666 = VERTEX_POINT ( 'NONE', #542 ) ;
#3667 = DIRECTION ( 'NONE',  ( 1.000000000000000000, -0.000000000000000000, -0.000000000000000000 ) ) ;
#3668 = DIRECTION ( 'NONE',  ( -1.000000000000000000, -3.469446951953614682E-16, -0.000000000000000000 ) ) ;
#3669 = EDGE_LOOP ( 'NONE', ( #18691, #13001, #20240, #11481 ) ) ;
#3670 = CARTESIAN_POINT ( 'NONE',  ( 112.7436279071538792, -91.18044947428829516, -90.00000000000000000 ) ) ;
#3671 = ADVANCED_FACE ( 'NONE', ( #15291 ), #8161, .F. ) ;
#3672 = DIRECTION ( 'NONE',  ( 3.469446951953614682E-16, -1.000000000000000000, 3.483493295888648978E-15 ) ) ;
#3673 = AXIS2_PLACEMENT_3D ( 'NONE', #18231, #10908, #20269 ) ;
#3674 = DIRECTION ( 'NONE',  ( 0.000000000000000000, -1.000000000000000000, 0.000000000000000000 ) ) ;
#3675 = DIRECTION ( 'NONE',  ( 1.110223024625155594E-14, 0.000000000000000000, -1.000000000000000000 ) ) ;
#3676 = CARTESIAN_POINT ( 'NONE',  ( 5.000000000000015099, 4.250000000000000000, 0.000000000000000000 ) ) ;
#3677 = EDGE_CURVE ( 'NONE', #2034, #5659, #4394, .T. ) ;
#3678 = CARTESIAN_POINT ( 'NONE',  ( 3.999999999999999112, 2.309401076758497595, -3.504271511726784194 ) ) ;
#3679 = CARTESIAN_POINT ( 'NONE',  ( 2.000000000000005329, -3.464101615137751722, 0.000000000000000000 ) ) ;
#3680 = VECTOR ( 'NONE', #11302, 1000.000000000000000 ) ;
#3681 = ORIENTED_EDGE ( 'NONE', *, *, #22989, .F. ) ;
#3682 = EDGE_LOOP ( 'NONE', ( #8085, #15317, #11499, #3557 ) ) ;
#3683 = CARTESIAN_POINT ( 'NONE',  ( -285.2000000000013529, -89.99999999999896261, -37.68333333333335844 ) ) ;
#3685 = CARTESIAN_POINT ( 'NONE',  ( 0.000000000000000000, 0.000000000000000000, 90.00000000000000000 ) ) ;
#3684 =( REPRESENTATION_RELATIONSHIP ('NONE','NONE', #10127, #11474 ) REPRESENTATION_RELATIONSHIP_WITH_TRANSFORMATION ( #8876 )SHAPE_REPRESENTATION_RELATIONSHIP( ) );
#3686 = EDGE_LOOP ( 'NONE', ( #14401, #21703, #12674, #4879 ) ) ;
#3687 = CYLINDRICAL_SURFACE ( 'NONE', #11234, 5.199999999999982414 ) ;
#3688 = CARTESIAN_POINT ( 'NONE',  ( 2.352174619736673744, -7.302225387959338399, -7.450218641350605076 ) ) ;
#3689 = CIRCLE ( 'NONE', #11858, 2.055000000000001492 ) ;
#3690 = ORIENTED_EDGE ( 'NONE', *, *, #5895, .T. ) ;
#3691 = FACE_OUTER_BOUND ( 'NONE', #20690, .T. ) ;
#3692 = DIRECTION ( 'NONE',  ( -6.676953772165163028E-17, -0.8660254037844398178, -0.4999999999999980016 ) ) ;
#3693 = VERTEX_POINT ( 'NONE', #15407 ) ;
#3694 = EDGE_CURVE ( 'NONE', #12407, #19135, #4150, .T. ) ;
#3695 = CARTESIAN_POINT ( 'NONE',  ( 45.00000000000002132, -56.79999999999935056, 140.0000000000001990 ) ) ;
#3696 = CARTESIAN_POINT ( 'NONE',  ( -4.000000000000000000, 1.941961291383472732, -0.3515519931180205448 ) ) ;
#3697 = CARTESIAN_POINT ( 'NONE',  ( 10.00000000000000000, -1.308996938995744097, 200.0000119999999981 ) ) ;
#3698 = ORIENTED_EDGE ( 'NONE', *, *, #4824, .F. ) ;
#3699 = CARTESIAN_POINT ( 'NONE',  ( 235.0000000000000284, -489.9999999999998863, 60.00000000000000000 ) ) ;
#3700 = CARTESIAN_POINT ( 'NONE',  ( -136.8329206786529539, -1072.813188689869321, 28.74044610054857074 ) ) ;
#3701 = ADVANCED_FACE ( 'NONE', ( #15054 ), #16582, .T. ) ;
#3702 = FACE_OUTER_BOUND ( 'NONE', #21428, .T. ) ;
#3703 = ORIENTED_EDGE ( 'NONE', *, *, #8396, .F. ) ;
#3704 = ORIENTED_EDGE ( 'NONE', *, *, #713, .T. ) ;
#3705 = CARTESIAN_POINT ( 'NONE',  ( 16.55500000000001393, 3.061616997868383634E-16, -2.500000000000000444 ) ) ;
#3706 = PRODUCT_CONTEXT ( 'NONE', #18458, 'mechanical' ) ;
#3707 = CARTESIAN_POINT ( 'NONE',  ( -127.1852154257917249, 88.59424271557217878, -32.17346063704740544 ) ) ;
#3708 = EDGE_CURVE ( 'NONE', #15482, #13840, #19117, .T. ) ;
#3709 = AXIS2_PLACEMENT_3D ( 'NONE', #16694, #20293, #22468 ) ;
#3710 = EDGE_CURVE ( 'NONE', #17062, #1715, #10615, .T. ) ;
#3711 = CYLINDRICAL_SURFACE ( 'NONE', #16171, 5.249999999999942268 ) ;
#3712 = DIRECTION ( 'NONE',  ( 1.000000000000000000, 0.000000000000000000, 0.000000000000000000 ) ) ;
#3713 = CARTESIAN_POINT ( 'NONE',  ( 70.00000000000000000, -87.33333333333332860, 3.000000000000001332 ) ) ;
#3714 = ORIENTED_EDGE ( 'NONE', *, *, #5895, .F. ) ;
#3715 = DIRECTION ( 'NONE',  ( 0.000000000000000000, 1.000000000000000000, -1.224646799147353207E-16 ) ) ;
#3716 = PRODUCT_DEFINITION_CONTEXT ( 'detailed design', #3636, 'design' ) ;
#3717 = VECTOR ( 'NONE', #15604, 1000.000000000000114 ) ;
#3718 = VERTEX_POINT ( 'NONE', #16971 ) ;
#3719 = CARTESIAN_POINT ( 'NONE',  ( 65.00000000000005684, -52.79999999999970584, 35.00000000000017764 ) ) ;
#3720 = DIRECTION ( 'NONE',  ( -1.000000000000000000, -0.000000000000000000, -0.000000000000000000 ) ) ;
#3721 = ORIENTED_EDGE ( 'NONE', *, *, #14896, .F. ) ;
#3722 = VECTOR ( 'NONE', #16400, 1000.000000000000000 ) ;
#3723 = DIRECTION ( 'NONE',  ( 0.000000000000000000, 0.000000000000000000, 1.000000000000000000 ) ) ;
#3724 = EDGE_LOOP ( 'NONE', ( #11287, #11752 ) ) ;
#3725 = EDGE_CURVE ( 'NONE', #19888, #17037, #434, .T. ) ;
#3726 = DIRECTION ( 'NONE',  ( 0.8191520442889902442, 1.003171929053522651E-16, -0.5735764363510482688 ) ) ;
#3727 = CARTESIAN_POINT ( 'NONE',  ( -4.175002511812151873, -2.208363329454905877, -3.469254087858246738 ) ) ;
#3728 = ORIENTED_EDGE ( 'NONE', *, *, #6097, .T. ) ;
#3729 = CARTESIAN_POINT ( 'NONE',  ( 34.99999999999999289, 90.00000000000000000, 0.000000000000000000 ) ) ;
#3730 = LINE ( 'NONE', #7483, #8110 ) ;
#3731 = EDGE_CURVE ( 'NONE', #20709, #23021, #16956, .T. ) ;
#3732 = CARTESIAN_POINT ( 'NONE',  ( 24.99999999999998224, -1001.636246173744667, 145.0000119999999697 ) ) ;
#3733 = EDGE_CURVE ( 'NONE', #15272, #1785, #17803, .T. ) ;
#3734 = VECTOR ( 'NONE', #2394, 1000.000000000000000 ) ;
#3735 = LINE ( 'NONE', #16913, #3380 ) ;
#3736 = CARTESIAN_POINT ( 'NONE',  ( -2.459698528280933161, 7.240146430416066536, -0.09933465333851029810 ) ) ;
#3737 = EDGE_CURVE ( 'NONE', #19135, #13502, #884, .T. ) ;
#3738 = PLANE ( 'NONE',  #11551 ) ;
#3739 = VERTEX_POINT ( 'NONE', #6929 ) ;
#3740 = DIRECTION ( 'NONE',  ( 1.000000000000000000, -3.491481338843133355E-15, 0.000000000000000000 ) ) ;
#3741 = VECTOR ( 'NONE', #7148, 1000.000000000000000 ) ;
#3742 = FACE_BOUND ( 'NONE', #15940, .T. ) ;
#3743 = CIRCLE ( 'NONE', #17628, 0.2000000000000000944 ) ;
#3745 = ORIENTED_EDGE ( 'NONE', *, *, #1516, .T. ) ;
#3744 = ORIENTED_EDGE ( 'NONE', *, *, #7934, .F. ) ;
#3746 = DIRECTION ( 'NONE',  ( 6.123233995736766036E-17, -1.000000000000000000, 0.000000000000000000 ) ) ;
#3747 = CARTESIAN_POINT ( 'NONE',  ( -136.5243927815879204, -1073.390114808523549, -28.00764941310471556 ) ) ;
#3748 = CARTESIAN_POINT ( 'NONE',  ( 280.1244294735509470, 273.0000000000000000, -145.6807971656550933 ) ) ;
#3749 = VERTEX_POINT ( 'NONE', #19717 ) ;
#3750 = CARTESIAN_POINT ( 'NONE',  ( -72.64999999999996305, -112.6666666666667140, 124.9999999999999858 ) ) ;
#3751 = ORIENTED_EDGE ( 'NONE', *, *, #10525, .T. ) ;
#3752 = AXIS2_PLACEMENT_3D ( 'NONE', #10984, #18303, #9147 ) ;
#3753 = DIRECTION ( 'NONE',  ( 0.000000000000000000, 0.000000000000000000, -1.000000000000000000 ) ) ;
#3754 = ORIENTED_EDGE ( 'NONE', *, *, #10151, .T. ) ;
#3755 = CIRCLE ( 'NONE', #17284, 7.499999999999998224 ) ;
#3756 = DIRECTION ( 'NONE',  ( -6.982962677686266711E-15, 0.000000000000000000, 1.000000000000000000 ) ) ;
#3757 = DIRECTION ( 'NONE',  ( -1.110223024625157172E-14, 0.000000000000000000, -1.000000000000000000 ) ) ;
#3758 = AXIS2_PLACEMENT_3D ( 'NONE', #20221, #81, #16737 ) ;
#3759 = VERTEX_POINT ( 'NONE', #22972 ) ;
#3760 = VECTOR ( 'NONE', #625, 1000.000000000000000 ) ;
#3761 = DIRECTION ( 'NONE',  ( 1.000000000000000000, 0.000000000000000000, 0.000000000000000000 ) ) ;
#3762 = EDGE_LOOP ( 'NONE', ( #17911, #2104, #2310, #10511 ) ) ;
#3763 = CARTESIAN_POINT ( 'NONE',  ( -282.2000000000007276, 75.00000000000100897, -90.00000000000000000 ) ) ;
#3764 = CARTESIAN_POINT ( 'NONE',  ( 145.0000000000000284, -500.0000000000000000, -32.49999999999997158 ) ) ;
#3765 = ADVANCED_FACE ( 'NONE', ( #21532 ), #13979, .T. ) ;
#3766 = CARTESIAN_POINT ( 'NONE',  ( 4.000000000000000000, 0.8378280264232961239, -3.220590601395640018 ) ) ;
#3767 = DIRECTION ( 'NONE',  ( -0.000000000000000000, -0.000000000000000000, 1.000000000000000000 ) ) ;
#3768 = CARTESIAN_POINT ( 'NONE',  ( 45.00000000000002132, -52.79999999999936477, 137.3500000000002217 ) ) ;
#3769 = DIRECTION ( 'NONE',  ( 1.000000000000000000, 0.000000000000000000, 0.000000000000000000 ) ) ;
#3770 = VERTEX_POINT ( 'NONE', #19840 ) ;
#3771 = DIRECTION ( 'NONE',  ( 1.000000000000000000, 0.000000000000000000, 0.000000000000000000 ) ) ;
#3772 = AXIS2_PLACEMENT_3D ( 'NONE', #1692, #14522, #5096 ) ;
#3773 = CARTESIAN_POINT ( 'NONE',  ( -44.99999999999997868, -56.79999999999937188, 142.6500000000001478 ) ) ;
#3774 = CIRCLE ( 'NONE', #10295, 24.99999999999998224 ) ;
#3775 = CARTESIAN_POINT ( 'NONE',  ( 3.000000000000002665, 0.000000000000000000, 0.000000000000000000 ) ) ;
#3776 = VECTOR ( 'NONE', #18332, 1000.000000000000000 ) ;
#3777 = ORIENTED_EDGE ( 'NONE', *, *, #8405, .F. ) ;
#3778 = AXIS2_PLACEMENT_3D ( 'NONE', #10990, #18309, #7338 ) ;
#3779 = CARTESIAN_POINT ( 'NONE',  ( 0.000000000000000000, 0.000000000000000000, -5.000000000000000888 ) ) ;
#3780 = DIRECTION ( 'NONE',  ( 0.000000000000000000, 0.000000000000000000, 1.000000000000000000 ) ) ;
#3781 = CARTESIAN_POINT ( 'NONE',  ( 7.500000000000002665, 3.988838049906435312, -0.8529248949437669980 ) ) ;
#3782 = DIRECTION ( 'NONE',  ( 0.000000000000000000, 0.5000000000000011102, 0.8660254037844380415 ) ) ;
#3783 = CARTESIAN_POINT ( 'NONE',  ( -280.3431883596742864, 273.0000000000000000, -145.0627246250092810 ) ) ;
#3784 = ORIENTED_EDGE ( 'NONE', *, *, #7127, .F. ) ;
#3785 = CARTESIAN_POINT ( 'NONE',  ( 146.0000000000002558, -801.0618695410406644, -32.05499999999356930 ) ) ;
#3786 = ORIENTED_EDGE ( 'NONE', *, *, #6661, .T. ) ;
#3788 = DIRECTION ( 'NONE',  ( -1.000000000000000000, -0.000000000000000000, -0.000000000000000000 ) ) ;
#3787 = AXIS2_PLACEMENT_3D ( 'NONE', #18219, #9303, #18563 ) ;
#3789 = DIRECTION ( 'NONE',  ( 0.000000000000000000, 0.000000000000000000, 1.000000000000000000 ) ) ;
#3791 = AXIS2_PLACEMENT_3D ( 'NONE', #10591, #8636, #16123 ) ;
#3790 = STYLED_ITEM ( 'NONE', ( #9208 ), #2073 ) ;
#3792 = AXIS2_PLACEMENT_3D ( 'NONE', #15641, #10462, #656 ) ;
#3793 = DIRECTION ( 'NONE',  ( -0.000000000000000000, 0.4999999999999979461, -0.8660254037844397068 ) ) ;
#3794 = ORIENTED_EDGE ( 'NONE', *, *, #185, .F. ) ;
#3795 = CONICAL_SURFACE ( 'NONE', #14266, 4.000000000000000000, 0.8911886515913786111 ) ;
#3796 = CARTESIAN_POINT ( 'NONE',  ( 135.4018704341561374, -51.87806360044677945, -2.775557561562891351E-14 ) ) ;
#3797 = EDGE_CURVE ( 'NONE', #12879, #9739, #1249, .T. ) ;
#3798 = PLANE ( 'NONE',  #16191 ) ;
#3799 = CARTESIAN_POINT ( 'NONE',  ( 45.00000000000002132, -52.79999999999935056, 192.3500000000002501 ) ) ;
#3800 = CARTESIAN_POINT ( 'NONE',  ( -7.549004593702459687, 4.358419834287835748, -7.700121441565839220 ) ) ;
#3801 = DIRECTION ( 'NONE',  ( 0.000000000000000000, -1.000000000000000000, 0.000000000000000000 ) ) ;
#3802 = EDGE_CURVE ( 'NONE', #4083, #11935, #4647, .T. ) ;
#3803 = CARTESIAN_POINT ( 'NONE',  ( -7.500000000000667910, 3.157052757790226316, -7.642767288269818771 ) ) ;
#3804 = ORIENTED_EDGE ( 'NONE', *, *, #12596, .F. ) ;
#3805 = ORIENTED_EDGE ( 'NONE', *, *, #305, .T. ) ;
#3806 = DIRECTION ( 'NONE',  ( 0.000000000000000000, 0.000000000000000000, -1.000000000000000000 ) ) ;
#3807 = CARTESIAN_POINT ( 'NONE',  ( 279.9999999999999432, 272.9999999999999432, 145.0000000000000284 ) ) ;
#3808 = EDGE_CURVE ( 'NONE', #6854, #15324, #5003, .T. ) ;
#3809 = EDGE_CURVE ( 'NONE', #9091, #4872, #2677, .T. ) ;
#3810 = ORIENTED_EDGE ( 'NONE', *, *, #18462, .T. ) ;
#3811 = COLOUR_RGB ( '',1.000000000000000000, 0.9490196078431372140, 0.9098039215686274384 ) ;
#3812 = CARTESIAN_POINT ( 'NONE',  ( 285.2000000000013529, -127.0000000000000568, 146.4928932188134638 ) ) ;
#3813 = CARTESIAN_POINT ( 'NONE',  ( 7.779103221381273414, -4.168986698926031131, -7.929128246061905472 ) ) ;
#3814 = VECTOR ( 'NONE', #2181, 1000.000000000000000 ) ;
#3816 = AXIS2_PLACEMENT_3D ( 'NONE', #23080, #1231, #12399 ) ;
#3815 = COLOUR_RGB ( '',1.000000000000000000, 0.9490196078431372140, 0.9098039215686274384 ) ;
#3817 = VECTOR ( 'NONE', #22769, 1000.000000000000000 ) ;
#3818 = TOROIDAL_SURFACE ( 'NONE', #6540, 24.69999999999999929, 0.3000000000000007661 ) ;
#3819 = AXIS2_PLACEMENT_3D ( 'NONE', #2296, #9690, #6285 ) ;
#3820 = CARTESIAN_POINT ( 'NONE',  ( 282.1999999999999318, 267.7999999999999545, -146.4928932188133786 ) ) ;
#3821 = AXIS2_PLACEMENT_3D ( 'NONE', #156, #16456, #22223 ) ;
#3822 = VECTOR ( 'NONE', #9293, 1000.000000000000000 ) ;
#3823 = ADVANCED_FACE ( 'NONE', ( #19590 ), #1129, .F. ) ;
#3824 = VERTEX_POINT ( 'NONE', #16112 ) ;
#3825 = DIRECTION ( 'NONE',  ( 1.000000000000000000, -0.000000000000000000, -9.860133695827843917E-17 ) ) ;
#3826 = DIRECTION ( 'NONE',  ( 0.000000000000000000, 0.000000000000000000, -1.000000000000000000 ) ) ;
#3827 = PLANE ( 'NONE',  #16196 ) ;
#3828 = EDGE_LOOP ( 'NONE', ( #13650, #12892, #17242, #8630 ) ) ;
#3829 = CARTESIAN_POINT ( 'NONE',  ( 2.500000000000000444, 0.000000000000000000, -5.000000000000000888 ) ) ;
#3830 = DIRECTION ( 'NONE',  ( 0.000000000000000000, -1.000000000000000000, -3.172065784643303781E-15 ) ) ;
#3831 = CARTESIAN_POINT ( 'NONE',  ( -6.473970235329672780E-16, -4.862606272033106691, -3.745885042887442395 ) ) ;
#3832 = EDGE_LOOP ( 'NONE', ( #9105, #6349 ) ) ;
#3833 = CARTESIAN_POINT ( 'NONE',  ( 7.914973979435151463, 3.817460047930444134, -7.907502498112419786 ) ) ;
#3834 = PRODUCT_CONTEXT ( 'NONE', #9845, 'mechanical' ) ;
#3835 = CARTESIAN_POINT ( 'NONE',  ( 0.000000000000000000, 0.000000000000000000, -100.0000000000000000 ) ) ;
#3837 = VECTOR ( 'NONE', #17919, 1000.000000000000000 ) ;
#3836 = AXIS2_PLACEMENT_3D ( 'NONE', #14318, #21397, #8609 ) ;
#3839 = CARTESIAN_POINT ( 'NONE',  ( -5.276498195231978272, 6.073236878017963747, -7.633618187056680604 ) ) ;
#3838 =( GEOMETRIC_REPRESENTATION_CONTEXT ( 3 ) GLOBAL_UNCERTAINTY_ASSIGNED_CONTEXT ( ( #13553 ) ) GLOBAL_UNIT_ASSIGNED_CONTEXT ( ( #9334, #14883, #5218 ) ) REPRESENTATION_CONTEXT ( 'NONE', 'WORKASPACE' ) );
#3840 = VECTOR ( 'NONE', #7258, 1000.000000000000000 ) ;
#3841 = CARTESIAN_POINT ( 'NONE',  ( 2.000000000000000444, 3.464101615137754830, -3.142992957459231018 ) ) ;
#3842 = VECTOR ( 'NONE', #9547, 1000.000000000000000 ) ;
#3843 = CIRCLE ( 'NONE', #20810, 5.384454397937118664 ) ;
#3844 = ORIENTED_EDGE ( 'NONE', *, *, #2754, .T. ) ;
#3845 = VERTEX_POINT ( 'NONE', #12524 ) ;
#3846 = DIRECTION ( 'NONE',  ( 0.000000000000000000, 1.000000000000000000, -3.495664435217746987E-15 ) ) ;
#3847 = ADVANCED_FACE ( 'NONE', ( #12418, #10696, #21659 ), #5115, .T. ) ;
#3848 = EDGE_CURVE ( 'NONE', #20062, #21409, #8378, .T. ) ;
#3849 = EDGE_CURVE ( 'NONE', #9726, #1322, #23504, .T. ) ;
#3850 = MANIFOLD_SOLID_BREP ( 'Hex', #964 ) ;
#3851 = CARTESIAN_POINT ( 'NONE',  ( -281.4928932188134354, 35.00000000000022737, 147.2000000000008413 ) ) ;
#3852 = EDGE_CURVE ( 'NONE', #18827, #22831, #11991, .T. ) ;
#3853 = CARTESIAN_POINT ( 'NONE',  ( 25.00000000000002132, -52.79999999999942162, 125.0000000000001990 ) ) ;
#3854 = EDGE_CURVE ( 'NONE', #9508, #18021, #6573, .T. ) ;
#3855 = ORIENTED_EDGE ( 'NONE', *, *, #19775, .T. ) ;
#3857 = EDGE_CURVE ( 'NONE', #11790, #19892, #5369, .T. ) ;
#3856 = CARTESIAN_POINT ( 'NONE',  ( 65.00000000000002842, -52.79999999999929372, 155.0000000000002274 ) ) ;
#3858 = MECHANICAL_DESIGN_GEOMETRIC_PRESENTATION_REPRESENTATION (  '', ( #3790 ), #11959 ) ;
#3859 = AXIS2_PLACEMENT_3D ( 'NONE', #14257, #5168, #17735 ) ;
#3860 = AXIS2_PLACEMENT_3D ( 'NONE', #9773, #9408, #22665 ) ;
#3861 = VECTOR ( 'NONE', #453, 1000.000000000000000 ) ;
#3862 = ORIENTED_EDGE ( 'NONE', *, *, #15221, .F. ) ;
#3863 = FACE_OUTER_BOUND ( 'NONE', #21133, .T. ) ;
#3864 = ORIENTED_EDGE ( 'NONE', *, *, #11275, .T. ) ;
#3865 = DIRECTION ( 'NONE',  ( -1.000000000000000000, 0.000000000000000000, 0.000000000000000000 ) ) ;
#3866 = CARTESIAN_POINT ( 'NONE',  ( -45.00000000000000000, 272.9999999999999432, 0.000000000000000000 ) ) ;
#3867 = CARTESIAN_POINT ( 'NONE',  ( -15.24974479720505371, -1019.877690639539082, 145.0000119999999697 ) ) ;
#3868 = DIRECTION ( 'NONE',  ( 0.000000000000000000, -0.000000000000000000, 1.000000000000000000 ) ) ;
#3869 = DIRECTION ( 'NONE',  ( 1.110223024625157172E-14, 0.000000000000000000, -1.000000000000000000 ) ) ;
#3870 = CARTESIAN_POINT ( 'NONE',  ( 0.000000000000000000, -129.2000000000000455, 7.690461757479017101E-15 ) ) ;
#3871 = VERTEX_POINT ( 'NONE', #23586 ) ;
#3872 = EDGE_CURVE ( 'NONE', #19527, #20235, #6195, .T. ) ;
#3873 = FACE_OUTER_BOUND ( 'NONE', #19383, .T. ) ;
#3874 = CARTESIAN_POINT ( 'NONE',  ( 281.4928932188134354, -132.2000000000000455, -7.703011046602857601E-15 ) ) ;
#3875 =( LENGTH_UNIT ( ) NAMED_UNIT ( * ) SI_UNIT ( .MILLI., .METRE. ) );
#3877 = ORIENTED_EDGE ( 'NONE', *, *, #18176, .T. ) ;
#3876 = EDGE_LOOP ( 'NONE', ( #2660, #20408 ) ) ;
#3878 = CARTESIAN_POINT ( 'NONE',  ( -293.2000000000010118, -90.00000000000017053, 24.33333333333259674 ) ) ;
#3879 = CARTESIAN_POINT ( 'NONE',  ( -136.3944205523264088, -1073.631384736298514, -27.82770220384456294 ) ) ;
#3880 = DIRECTION ( 'NONE',  ( -0.000000000000000000, -0.000000000000000000, 1.000000000000000000 ) ) ;
#3881 = EDGE_LOOP ( 'NONE', ( #19327, #2633, #15079, #19810 ) ) ;
#3882 = CARTESIAN_POINT ( 'NONE',  ( -134.6768122279365798, -1076.727833257003567, 28.88700448195638515 ) ) ;
#3883 = EDGE_CURVE ( 'NONE', #22438, #17622, #9242, .T. ) ;
#3884 = ADVANCED_FACE ( 'NONE', ( #16345 ), #4992, .F. ) ;
#3885 = EDGE_LOOP ( 'NONE', ( #23721, #7361 ) ) ;
#3886 = ADVANCED_FACE ( 'NONE', ( #12877 ), #13139, .F. ) ;
#3887 = CARTESIAN_POINT ( 'NONE',  ( 5.200000000000002842, 0.000000000000000000, 0.000000000000000000 ) ) ;
#3888 = ORIENTED_EDGE ( 'NONE', *, *, #10067, .F. ) ;
#3889 = LINE ( 'NONE', #1827, #19244 ) ;
#3890 = DIRECTION ( 'NONE',  ( 0.000000000000000000, -1.000000000000000000, 0.000000000000000000 ) ) ;
#3891 = ITEM_DEFINED_TRANSFORMATION ( 'NONE', 'NONE', #410,  #11210 ) ;
#3892 = ORIENTED_EDGE ( 'NONE', *, *, #14111, .T. ) ;
#3893 = LINE ( 'NONE', #21247, #3680 ) ;
#3894 = ORIENTED_EDGE ( 'NONE', *, *, #23803, .T. ) ;
#3895 = LINE ( 'NONE', #18264, #12893 ) ;
#3896 = CARTESIAN_POINT ( 'NONE',  ( 0.2727178028658734932, 2.726369936601794865E-15, -21.02499999999999503 ) ) ;
#3897 = LINE ( 'NONE', #20550, #18071 ) ;
#3898 = DIRECTION ( 'NONE',  ( 0.000000000000000000, 0.000000000000000000, -1.000000000000000000 ) ) ;
#3899 = CARTESIAN_POINT ( 'NONE',  ( -280.4976310729378497, 272.3699028110927429, -147.6339272673398000 ) ) ;
#3900 = DIRECTION ( 'NONE',  ( 0.000000000000000000, 0.5000000000000012212, 0.8660254037844380415 ) ) ;
#3901 = ORIENTED_EDGE ( 'NONE', *, *, #9449, .T. ) ;
#3902 = CARTESIAN_POINT ( 'NONE',  ( 0.000000000000000000, 0.000000000000000000, 0.000000000000000000 ) ) ;
#3903 = DIRECTION ( 'NONE',  ( -0.000000000000000000, -0.000000000000000000, 1.000000000000000000 ) ) ;
#3904 = DIRECTION ( 'NONE',  ( 0.000000000000000000, 0.000000000000000000, -1.000000000000000000 ) ) ;
#3905 = CARTESIAN_POINT ( 'NONE',  ( 281.1079617568158824, 269.7223300543793698, 145.4976310729378497 ) ) ;
#3906 = DIRECTION ( 'NONE',  ( 1.000000000000000000, 0.000000000000000000, 0.000000000000000000 ) ) ;
#3907 = CARTESIAN_POINT ( 'NONE',  ( 126.3653543294818178, 77.28387428943173632, -29.99999999999356604 ) ) ;
#3908 = CARTESIAN_POINT ( 'NONE',  ( -282.2000000000013529, -89.99999999999896261, -37.68333333333335844 ) ) ;
#3909 = VERTEX_POINT ( 'NONE', #18258 ) ;
#3910 = FACE_OUTER_BOUND ( 'NONE', #7681, .T. ) ;
#3911 = EDGE_LOOP ( 'NONE', ( #13777, #1597 ) ) ;
#3912 = DIRECTION ( 'NONE',  ( 0.000000000000000000, 0.000000000000000000, 1.000000000000000000 ) ) ;
#3913 = SURFACE_SIDE_STYLE ('',( #8690 ) ) ;
#3914 = DIRECTION ( 'NONE',  ( 0.000000000000000000, 1.000000000000000000, -1.103561164596346103E-15 ) ) ;
#3915 = ORIENTED_EDGE ( 'NONE', *, *, #15028, .T. ) ;
#3916 = CARTESIAN_POINT ( 'NONE',  ( 0.000000000000000000, -74.99999999999970157, 129.9038105676659711 ) ) ;
#3917 = FACE_OUTER_BOUND ( 'NONE', #19588, .T. ) ;
#3918 = CARTESIAN_POINT ( 'NONE',  ( 10.00000000000000000, 6.613092715395708453E-16, 5.400000000000002132 ) ) ;
#3919 = CYLINDRICAL_SURFACE ( 'NONE', #19024, 2.500000000000002220 ) ;
#3920 = LINE ( 'NONE', #12916, #23067 ) ;
#3921 = CARTESIAN_POINT ( 'NONE',  ( -4.000000000000000000, -0.3979232138631226823, -3.896351557369779711E-17 ) ) ;
#3922 = CARTESIAN_POINT ( 'NONE',  ( -20.63749999999999574, 0.000000000000000000, 0.000000000000000000 ) ) ;
#3923 = ORIENTED_EDGE ( 'NONE', *, *, #16663, .T. ) ;
#3924 = SHAPE_REPRESENTATION_RELATIONSHIP ( 'NONE' , 'NONE' ,  #3124, #22256 ) ;
#3925 = DIRECTION ( 'NONE',  ( 1.000000000000000000, -0.000000000000000000, 6.982962677686266711E-15 ) ) ;
#3926 = DIRECTION ( 'NONE',  ( -0.000000000000000000, -0.000000000000000000, 1.000000000000000000 ) ) ;
#3927 = ORIENTED_EDGE ( 'NONE', *, *, #1439, .T. ) ;
#3928 = EDGE_CURVE ( 'NONE', #12485, #6553, #1828, .T. ) ;
#3929 = AXIS2_PLACEMENT_3D ( 'NONE', #16439, #14643, #15000 ) ;
#3931 = B_SPLINE_CURVE_WITH_KNOTS ( 'NONE', 3,
 ( #17164, #9563, #12984, #2307, #13462, #15249, #20775, #2054, #13106, #11653, #144, #3983, #20418, #624, #14769, #18958, #5931, #22102, #507, #7757, #9698, #17052, #5573, #14888, #3747, #3879, #2422, #11163, #18492, #16803, #1949, #22583 ),
 .UNSPECIFIED., .F., .F.,
 ( 4, 2, 2, 2, 2, 2, 2, 2, 2, 2, 2, 2, 2, 2, 2, 4 ),
 ( 0.000000000000000000, 0.0004914281572963174896, 0.0009828563145926349793, 0.001474284471888952361, 0.001965712629185269959, 0.002457140786481587773, 0.002948568943777904721, 0.003931425258370744615, 0.004422853415667163043, 0.004914281572963582340, 0.005405709730260000768, 0.005897137887556419197, 0.006388566044852838494, 0.006879994202149256922, 0.007371422359445676219, 0.007862850516742094648 ),
 .UNSPECIFIED. ) ;
#3930 = DIRECTION ( 'NONE',  ( 0.000000000000000000, -1.000000000000000000, 0.000000000000000000 ) ) ;
#3932 = DIRECTION ( 'NONE',  ( -1.000000000000000000, -0.000000000000000000, -0.000000000000000000 ) ) ;
#3933 = CARTESIAN_POINT ( 'NONE',  ( 2.500000000000000000, 2.357898499370433054, -1.951563910473907981E-15 ) ) ;
#3934 = EDGE_CURVE ( 'NONE', #12627, #22432, #11178, .T. ) ;
#3935 = ORIENTED_EDGE ( 'NONE', *, *, #8444, .F. ) ;
#3936 = CARTESIAN_POINT ( 'NONE',  ( 0.000000000000000000, 1.178949249685213863, -2.042000000000001148 ) ) ;
#3937 = DIRECTION ( 'NONE',  ( 0.000000000000000000, 1.000000000000000000, 4.183096374613631247E-18 ) ) ;
#3938 = EDGE_CURVE ( 'NONE', #17297, #23365, #5770, .T. ) ;
#3939 = DIRECTION ( 'NONE',  ( 0.000000000000000000, -0.8660254037844391517, -0.4999999999999991673 ) ) ;
#3940 = ORIENTED_EDGE ( 'NONE', *, *, #18670, .T. ) ;
#3941 = CARTESIAN_POINT ( 'NONE',  ( 7.499999999999999112, 0.000000000000000000, -100.0000000000000000 ) ) ;
#3942 = DIRECTION ( 'NONE',  ( -0.000000000000000000, 1.000000000000000000, 0.000000000000000000 ) ) ;
#3943 = EDGE_CURVE ( 'NONE', #16453, #3139, #14780, .T. ) ;
#3944 = ORIENTED_EDGE ( 'NONE', *, *, #20619, .F. ) ;
#3945 = CARTESIAN_POINT ( 'NONE',  ( 194.7500000000001990, -210.0000000000003411, -29.99999999999322498 ) ) ;
#3946 = SHAPE_DEFINITION_REPRESENTATION ( #14440, #8987 ) ;
#3947 = DIRECTION ( 'NONE',  ( -1.000000000000000000, 0.000000000000000000, -0.000000000000000000 ) ) ;
#3948 = DIRECTION ( 'NONE',  ( -1.000000000000000000, 0.000000000000000000, 0.000000000000000000 ) ) ;
#3949 = ORIENTED_EDGE ( 'NONE', *, *, #8706, .F. ) ;
#3950 = ORIENTED_EDGE ( 'NONE', *, *, #21410, .F. ) ;
#3951 = CARTESIAN_POINT ( 'NONE',  ( -129.2206655591611764, -1072.408698320350140, -29.99999999999356604 ) ) ;
#3952 = PLANE ( 'NONE',  #22944 ) ;
#3953 = PRODUCT_DEFINITION_CONTEXT ( 'detailed design', #14346, 'design' ) ;
#3954 = CONICAL_SURFACE ( 'NONE', #8620, 2.041999999999999815, 1.047197551196591858 ) ;
#3955 = APPLICATION_CONTEXT ( 'automotive_design' ) ;
#3956 = CARTESIAN_POINT ( 'NONE',  ( 60.00000000000000000, 0.000000000000000000, 3.000000000000000000 ) ) ;
#3957 = CYLINDRICAL_SURFACE ( 'NONE', #9933, 2.649999999999971934 ) ;
#3958 = EDGE_LOOP ( 'NONE', ( #23510, #8785, #8693, #9032 ) ) ;
#3959 = CARTESIAN_POINT ( 'NONE',  ( -288.2000000000006708, 90.00000000000102318, -35.00000000000001421 ) ) ;
#3960 = EDGE_CURVE ( 'NONE', #19049, #18989, #9619, .T. ) ;
#3961 = ORIENTED_EDGE ( 'NONE', *, *, #5807, .T. ) ;
#3962 = FACE_OUTER_BOUND ( 'NONE', #3881, .T. ) ;
#3963 = EDGE_CURVE ( 'NONE', #8364, #436, #7509, .T. ) ;
#3964 = PLANE ( 'NONE',  #17502 ) ;
#3965 = VERTEX_POINT ( 'NONE', #22112 ) ;
#3966 = CARTESIAN_POINT ( 'NONE',  ( -129.3084827928272205, 85.46529914716386145, -29.66799569545555215 ) ) ;
#3967 = VECTOR ( 'NONE', #23784, 1000.000000000000000 ) ;
#3968 = EDGE_CURVE ( 'NONE', #17073, #15945, #7270, .T. ) ;
#3969 = DIRECTION ( 'NONE',  ( -1.000000000000000000, 1.408839003528726857E-14, 6.982962677686266711E-15 ) ) ;
#3970 = CONICAL_SURFACE ( 'NONE', #5914, 10.39117206796836079, 1.221730476396047926 ) ;
#3971 = DIRECTION ( 'NONE',  ( -1.000000000000000000, 0.000000000000000000, 0.000000000000000000 ) ) ;
#3972 = DIRECTION ( 'NONE',  ( 0.000000000000000000, 0.000000000000000000, -1.000000000000000000 ) ) ;
#3973 = CARTESIAN_POINT ( 'NONE',  ( -79.99999999999994316, -59.79999999999918714, 250.0000000000000000 ) ) ;
#3974 = CARTESIAN_POINT ( 'NONE',  ( -85.22886158240795851, -117.3074641843678876, -90.00000000000000000 ) ) ;
#3975 = EDGE_CURVE ( 'NONE', #19949, #4882, #11195, .T. ) ;
#3976 = DIRECTION ( 'NONE',  ( -0.000000000000000000, -0.000000000000000000, 1.000000000000000000 ) ) ;
#3977 = VERTEX_POINT ( 'NONE', #22231 ) ;
#3978 = DIRECTION ( 'NONE',  ( 0.000000000000000000, 0.000000000000000000, -1.000000000000000000 ) ) ;
#3979 = LINE ( 'NONE', #11159, #20298 ) ;
#3980 = FILL_AREA_STYLE_COLOUR ( '', #16226 ) ;
#3982 = VERTEX_POINT ( 'NONE', #5470 ) ;
#3981 = ORIENTED_EDGE ( 'NONE', *, *, #18005, .T. ) ;
#3983 = CARTESIAN_POINT ( 'NONE',  ( -136.8329206786532097, -1072.813188689868639, -31.25955389945148966 ) ) ;
#3984 = CARTESIAN_POINT ( 'NONE',  ( 146.0000000000002274, -210.0000000000003411, -29.99999999999356604 ) ) ;
#3985 = VERTEX_POINT ( 'NONE', #21769 ) ;
#3986 = VECTOR ( 'NONE', #10399, 1000.000000000000000 ) ;
#3987 = CARTESIAN_POINT ( 'NONE',  ( 5.000000000000000000, 3.513898075855363068, 2.028749999999996945 ) ) ;
#3988 = AXIS2_PLACEMENT_3D ( 'NONE', #15544, #17350, #4660 ) ;
#3989 = EDGE_LOOP ( 'NONE', ( #21774, #10519, #8095, #13614 ) ) ;
#3990 = CARTESIAN_POINT ( 'NONE',  ( 0.000000000000000000, 0.000000000000000000, -9.449444346342714240 ) ) ;
#3991 = EDGE_LOOP ( 'NONE', ( #8643, #19958, #17018, #19670, #20568 ) ) ;
#3992 = EDGE_CURVE ( 'NONE', #22350, #13630, #23092, .T. ) ;
#3993 = CARTESIAN_POINT ( 'NONE',  ( 145.9999999999998010, -801.0618695410399823, 30.00000000000641620 ) ) ;
#3994 = SURFACE_STYLE_USAGE ( .BOTH. , #17179 ) ;
#3995 = ITEM_DEFINED_TRANSFORMATION ( 'NONE', 'NONE', #4645,  #11210 ) ;
#3996 = ORIENTED_EDGE ( 'NONE', *, *, #6944, .F. ) ;
#3997 = DIRECTION ( 'NONE',  ( 0.6964005597823107463, -0.7176533009294141507, 6.982962677686266711E-15 ) ) ;
#3998 = EDGE_LOOP ( 'NONE', ( #17400, #15518 ) ) ;
#3999 = CARTESIAN_POINT ( 'NONE',  ( -128.7674363984959598, 86.27842408395231644, 28.00959664470845567 ) ) ;
#4000 = LINE ( 'NONE', #13608, #10803 ) ;
#4001 = FACE_OUTER_BOUND ( 'NONE', #12359, .T. ) ;
#4002 = CIRCLE ( 'NONE', #1698, 155.0000000000000284 ) ;
#4003 = VECTOR ( 'NONE', #3767, 1000.000000000000000 ) ;
#4004 = FACE_OUTER_BOUND ( 'NONE', #22363, .T. ) ;
#4005 = EDGE_CURVE ( 'NONE', #1528, #12933, #5235, .T. ) ;
#4006 = ORIENTED_EDGE ( 'NONE', *, *, #10763, .F. ) ;
#4007 = CARTESIAN_POINT ( 'NONE',  ( -280.1244266425809428, 269.9697000000000457, -145.2840560642351875 ) ) ;
#4008 = ADVANCED_FACE ( 'NONE', ( #3408 ), #2432, .F. ) ;
#4009 = SURFACE_STYLE_USAGE ( .BOTH. , #4270 ) ;
#4010 = AXIS2_PLACEMENT_3D ( 'NONE', #5172, #9286, #20011 ) ;
#4011 = VERTEX_POINT ( 'NONE', #13712 ) ;
#4012 = DIRECTION ( 'NONE',  ( 0.000000000000000000, 0.000000000000000000, 1.000000000000000000 ) ) ;
#4013 = DIRECTION ( 'NONE',  ( -1.000000000000000000, 0.000000000000000000, 0.000000000000000000 ) ) ;
#4014 = CARTESIAN_POINT ( 'NONE',  ( 146.4450000000002206, -210.0000000000003411, -29.99999999999356248 ) ) ;
#4015 = CARTESIAN_POINT ( 'NONE',  ( 282.1696999999999775, 268.0840560642351988, 146.3684665762324926 ) ) ;
#4016 = CARTESIAN_POINT ( 'NONE',  ( -285.2000000000000455, 267.7999999999999545, -146.4928932188134354 ) ) ;
#4017 =( BOUNDED_SURFACE ( )  B_SPLINE_SURFACE ( 3, 2, ( 
 ( #1318, #1569, #5433 ),
 ( #8951, #20145, #12368 ),
 ( #10413, #17764, #1209 ),
 ( #8580, #6760, #21487 ),
 ( #19680, #8699, #3839 ),
 ( #11256, #3591, #13196 ),
 ( #20499, #11479, #15212 ),
 ( #7359, #22185, #13302 ) ),
 .UNSPECIFIED., .F., .F., .T. ) 
 B_SPLINE_SURFACE_WITH_KNOTS ( ( 4, 2, 2, 4 ),
 ( 3, 3 ),
 ( 0.03861844051980969916, 0.04325213341840641879, 0.04556897986770477860, 0.04788582631700313841 ),
 ( 0.000000000000000000, 1.000000000000000000 ),
 .UNSPECIFIED. ) 
 GEOMETRIC_REPRESENTATION_ITEM ( )  RATIONAL_B_SPLINE_SURFACE ( (
 ( 1.000000000000000000, 0.8047781759831920123, 1.000000000000000000),
 ( 1.000000000000000000, 0.8123762462803147955, 1.000000000000000000),
 ( 1.000000000000000000, 0.8190659850619289584, 1.000000000000000000),
 ( 1.000000000000000000, 0.8191937571012362085, 1.000000000000000000),
 ( 1.000000000000000000, 0.8176092952779873135, 1.000000000000000000),
 ( 1.000000000000000000, 0.8122962088597077690, 1.000000000000000000),
 ( 1.000000000000000000, 0.8086311330827508081, 1.000000000000000000),
 ( 1.000000000000000000, 0.8047712282214326551, 1.000000000000000000) ) ) 
 REPRESENTATION_ITEM ( '' )  SURFACE ( )  );
#4018 = CIRCLE ( 'NONE', #12573, 2.499999999999998668 ) ;
#4019 = CARTESIAN_POINT ( 'NONE',  ( -281.4928932188134354, -127.0000000000000568, -152.4000000000012847 ) ) ;
#4020 = CARTESIAN_POINT ( 'NONE',  ( 122.9957307409594449, -1094.324181863848480, 30.65186413114633268 ) ) ;
#4021 = ITEM_DEFINED_TRANSFORMATION ( 'NONE', 'NONE', #13925,  #11210 ) ;
#4022 = ORIENTED_EDGE ( 'NONE', *, *, #6374, .F. ) ;
#4023 = VECTOR ( 'NONE', #14170, 1000.000000000000000 ) ;
#4024 = DIRECTION ( 'NONE',  ( 0.000000000000000000, 0.000000000000000000, -1.000000000000000000 ) ) ;
#4025 = VERTEX_POINT ( 'NONE', #2182 ) ;
#4026 = VECTOR ( 'NONE', #15085, 1000.000000000000114 ) ;
#4027 = DIRECTION ( 'NONE',  ( 1.000000000000000000, 3.469446951953626515E-16, 3.469446951953613203E-16 ) ) ;
#4028 = CARTESIAN_POINT ( 'NONE',  ( 0.000000000000000000, 0.000000000000000000, 0.000000000000000000 ) ) ;
#4029 = LINE ( 'NONE', #18757, #6734 ) ;
#4030 = EDGE_LOOP ( 'NONE', ( #6266, #7502, #10158, #12104 ) ) ;
#4031 = CARTESIAN_POINT ( 'NONE',  ( -77.72886158240878274, 117.3074641843673049, -90.00000000000000000 ) ) ;
#4032 = CARTESIAN_POINT ( 'NONE',  ( 279.9999999999999432, 269.9999999999999432, 145.0000000000000284 ) ) ;
#4033 = DIRECTION ( 'NONE',  ( 1.000000000000000000, -0.000000000000000000, -0.000000000000000000 ) ) ;
#4034 = DIRECTION ( 'NONE',  ( 1.110223024625155594E-14, 0.000000000000000000, -1.000000000000000000 ) ) ;
#4035 = EDGE_CURVE ( 'NONE', #2736, #3058, #406, .T. ) ;
#4036 = DIRECTION ( 'NONE',  ( 0.6964005597823107463, -0.7176533009294141507, 6.982962677686266711E-15 ) ) ;
#4037 = AXIS2_PLACEMENT_3D ( 'NONE', #15336, #22551, #16889 ) ;
#4038 = DIRECTION ( 'NONE',  ( -0.000000000000000000, -0.000000000000000000, -1.000000000000000000 ) ) ;
#4039 = MANIFOLD_SOLID_BREP ( 'EndChamfer', #14496 ) ;
#4040 = AXIS2_PLACEMENT_3D ( 'NONE', #20357, #4503, #16645 ) ;
#4041 = EDGE_CURVE ( 'NONE', #22474, #22000, #1120, .T. ) ;
#4042 = EDGE_LOOP ( 'NONE', ( #10881, #6091, #18981, #7100 ) ) ;
#4043 = DIRECTION ( 'NONE',  ( 1.110223024625155594E-14, 0.000000000000000000, -1.000000000000000000 ) ) ;
#4044 = DIRECTION ( 'NONE',  ( -0.000000000000000000, -0.000000000000000000, 1.000000000000000000 ) ) ;
#4045 = VERTEX_POINT ( 'NONE', #11299 ) ;
#4046 = VECTOR ( 'NONE', #20463, 1000.000000000000000 ) ;
#4047 = VERTEX_POINT ( 'NONE', #750 ) ;
#4048 = CYLINDRICAL_SURFACE ( 'NONE', #2653, 160.0000000000000000 ) ;
#4049 = DIRECTION ( 'NONE',  ( 0.000000000000000000, 0.000000000000000000, 1.000000000000000000 ) ) ;
#4050 = DIRECTION ( 'NONE',  ( 1.302872740555339390E-32, -4.694093751100962712E-16, 1.000000000000000000 ) ) ;
#4051 = ORIENTED_EDGE ( 'NONE', *, *, #1025, .F. ) ;
#4052 = AXIS2_PLACEMENT_3D ( 'NONE', #12201, #3095, #14117 ) ;
#4053 = CARTESIAN_POINT ( 'NONE',  ( -2.000000000000007550, -3.464101615137749945, 0.000000000000000000 ) ) ;
#4054 = CARTESIAN_POINT ( 'NONE',  ( 1.500000000000001332, 0.000000000000000000, 8.000000000000000000 ) ) ;
#4055 = DIRECTION ( 'NONE',  ( 1.000000000000000000, 0.000000000000000000, 0.000000000000000000 ) ) ;
#4056 = VERTEX_POINT ( 'NONE', #16813 ) ;
#4057 = CARTESIAN_POINT ( 'NONE',  ( -31.74999999999995737, 5.204748896376250699E-16, -4.250000000000000000 ) ) ;
#4058 = AXIS2_PLACEMENT_3D ( 'NONE', #14297, #1090, #15857 ) ;
#4059 = DIRECTION ( 'NONE',  ( 0.000000000000000000, 0.000000000000000000, 1.000000000000000000 ) ) ;
#4060 = DIRECTION ( 'NONE',  ( 0.000000000000000000, 2.618450529776326854E-15, 1.000000000000000000 ) ) ;
#4061 = ORIENTED_EDGE ( 'NONE', *, *, #22012, .T. ) ;
#4062 = EDGE_CURVE ( 'NONE', #23038, #15253, #4206, .T. ) ;
#4063 = CARTESIAN_POINT ( 'NONE',  ( 0.000000000000000000, 0.000000000000000000, 0.000000000000000000 ) ) ;
#4064 = AXIS2_PLACEMENT_3D ( 'NONE', #22627, #11934, #21064 ) ;
#4065 = APPLICATION_PROTOCOL_DEFINITION ( 'draft international standard', 'automotive_design', 1998, #19698 ) ;
#4066 = ADVANCED_FACE ( 'NONE', ( #7627 ), #19087, .F. ) ;
#4067 = FACE_OUTER_BOUND ( 'NONE', #16357, .T. ) ;
#4068 = LINE ( 'NONE', #14973, #19207 ) ;
#4069 = DIRECTION ( 'NONE',  ( 1.000000000000000000, 0.000000000000000000, 0.000000000000000000 ) ) ;
#4070 = ADVANCED_FACE ( 'NONE', ( #22365 ), #13238, .F. ) ;
#4071 = EDGE_LOOP ( 'NONE', ( #22235, #7183, #21719, #11095, #23459 ) ) ;
#4072 = ORIENTED_EDGE ( 'NONE', *, *, #2683, .F. ) ;
#4073 = DIRECTION ( 'NONE',  ( -0.5114233182937522049, 0.4883095222350258280, -0.7071067811865532349 ) ) ;
#4074 = CARTESIAN_POINT ( 'NONE',  ( -69.99999999999997158, -87.33333333333338544, 0.000000000000000000 ) ) ;
#4075 = ADVANCED_FACE ( 'NONE', ( #8134 ), #22476, .F. ) ;
#4077 = ORIENTED_EDGE ( 'NONE', *, *, #10372, .F. ) ;
#4076 = MANIFOLD_SOLID_BREP ( 'Hex', #15270 ) ;
#4078 = DIRECTION ( 'NONE',  ( -2.238759164535664589E-46, -3.469446951953614189E-15, -1.000000000000000000 ) ) ;
#4080 = CARTESIAN_POINT ( 'NONE',  ( 45.00000000000004974, -56.79999999999964189, 107.6500000000002188 ) ) ;
#4079 = B_SPLINE_CURVE_WITH_KNOTS ( 'NONE', 3,
 ( #3235, #21619, #10531, #17617, #1205, #14037, #4708, #951, #17864, #6873, #19672, #12234, #19539, #3133, #1071, #8457, #23287, #19416, #12594, #10402, #2994, #12486, #21484, #19787, #8694, #10648, #8576, #6514, #5074, #12118, #21257, #17501 ),
 .UNSPECIFIED., .F., .F.,
 ( 4, 2, 2, 2, 2, 2, 2, 2, 2, 2, 2, 2, 2, 2, 2, 4 ),
 ( 0.000000000000000000, 0.0004914281572963870954, 0.0009828563145927741908, 0.001474284471889161178, 0.001965712629185548382, 0.002457140786481935586, 0.002948568943778322356, 0.003931425258371092427, 0.004422853415667472692, 0.004914281572963852956, 0.005405709730260233221, 0.005897137887556612619, 0.006388566044852993751, 0.006879994202149373149, 0.007371422359445754281, 0.007862850516742132811 ),
 .UNSPECIFIED. ) ;
#4081 = ORIENTED_EDGE ( 'NONE', *, *, #18682, .F. ) ;
#4082 = DIRECTION ( 'NONE',  ( 0.000000000000000000, 0.000000000000000000, -1.000000000000000000 ) ) ;
#4083 = VERTEX_POINT ( 'NONE', #19558 ) ;
#4084 = AXIS2_PLACEMENT_3D ( 'NONE', #13732, #21052, #4510 ) ;
#4085 = CARTESIAN_POINT ( 'NONE',  ( 100.0000000000000000, -1400.000000000000000, -145.0000000000001705 ) ) ;
#4086 = CARTESIAN_POINT ( 'NONE',  ( -4.000000000000000000, 0.000000000000000000, 0.000000000000000000 ) ) ;
#4087 = ORIENTED_EDGE ( 'NONE', *, *, #16821, .F. ) ;
#4088 = ORIENTED_EDGE ( 'NONE', *, *, #11255, .T. ) ;
#4089 = CARTESIAN_POINT ( 'NONE',  ( -0.1410422978106123659, 4.700232962125094893, -3.687027686973624707 ) ) ;
#4090 = CARTESIAN_POINT ( 'NONE',  ( -20.63749999999999574, 0.000000000000000000, 0.000000000000000000 ) ) ;
#4091 = AXIS2_PLACEMENT_3D ( 'NONE', #15289, #22620, #11433 ) ;
#4092 = DIRECTION ( 'NONE',  ( -0.000000000000000000, 1.000000000000000000, -0.000000000000000000 ) ) ;
#4093 = CARTESIAN_POINT ( 'NONE',  ( 0.000000000000000000, 0.000000000000000000, 0.000000000000000000 ) ) ;
#4094 = CARTESIAN_POINT ( 'NONE',  ( 52.00000000000000711, -131.9709811566878273, 2.168404344971008868E-15 ) ) ;
#4095 = DIRECTION ( 'NONE',  ( 1.000000000000000000, 0.000000000000000000, 0.000000000000000000 ) ) ;
#4096 = EDGE_CURVE ( 'NONE', #17932, #471, #22546, .T. ) ;
#4097 = LINE ( 'NONE', #17046, #746 ) ;
#4098 = ORIENTED_EDGE ( 'NONE', *, *, #14078, .T. ) ;
#4099 = EDGE_CURVE ( 'NONE', #13534, #13282, #972, .T. ) ;
#4100 = FACE_BOUND ( 'NONE', #5634, .T. ) ;
#4101 = DIRECTION ( 'NONE',  ( 0.000000000000000000, 0.000000000000000000, 1.000000000000000000 ) ) ;
#4102 = AXIS2_PLACEMENT_3D ( 'NONE', #5130, #7611, #15005 ) ;
#4103 = EDGE_LOOP ( 'NONE', ( #8311, #3351, #19843, #1700 ) ) ;
#4104 = LINE ( 'NONE', #6045, #2309 ) ;
#4105 = AXIS2_PLACEMENT_3D ( 'NONE', #20043, #16318, #9063 ) ;
#4106 = CARTESIAN_POINT ( 'NONE',  ( 281.3684637172358975, 268.4847249064869175, -150.2299999999999329 ) ) ;
#4107 = EDGE_CURVE ( 'NONE', #3666, #12421, #4492, .T. ) ;
#4108 = ORIENTED_EDGE ( 'NONE', *, *, #5599, .F. ) ;
#4109 = EDGE_CURVE ( 'NONE', #11121, #15263, #8595, .T. ) ;
#4110 = DIRECTION ( 'NONE',  ( -1.350636282998972974E-14, 0.000000000000000000, -1.000000000000000000 ) ) ;
#4111 = ORIENTED_EDGE ( 'NONE', *, *, #13335, .T. ) ;
#4112 = CIRCLE ( 'NONE', #17621, 23.97500000000000142 ) ;
#4113 = DIRECTION ( 'NONE',  ( 1.000000000000000000, -0.000000000000000000, 6.982962677686266711E-15 ) ) ;
#4114 = VERTEX_POINT ( 'NONE', #14301 ) ;
#4115 = ADVANCED_FACE ( 'NONE', ( #8484 ), #21150, .F. ) ;
#4116 = LINE ( 'NONE', #11526, #3814 ) ;
#4117 = CARTESIAN_POINT ( 'NONE',  ( 0.000000000000000000, 0.000000000000000000, 0.000000000000000000 ) ) ;
#4118 = AXIS2_PLACEMENT_3D ( 'NONE', #19766, #12217, #10143 ) ;
#4119 = ORIENTED_EDGE ( 'NONE', *, *, #15493, .F. ) ;
#4120 = FACE_OUTER_BOUND ( 'NONE', #14104, .T. ) ;
#4121 = ORIENTED_EDGE ( 'NONE', *, *, #15583, .T. ) ;
#4122 = AXIS2_PLACEMENT_3D ( 'NONE', #23776, #7233, #21971 ) ;
#4123 = DIRECTION ( 'NONE',  ( -0.000000000000000000, 1.000000000000000000, -0.000000000000000000 ) ) ;
#4124 = AXIS2_PLACEMENT_3D ( 'NONE', #9441, #16795, #16684 ) ;
#4125 = CARTESIAN_POINT ( 'NONE',  ( -4.211140560182196957, 2.431303136016537803, -3.745885042887433514 ) ) ;
#4126 = DIRECTION ( 'NONE',  ( -0.000000000000000000, -0.000000000000000000, 1.000000000000000000 ) ) ;
#4127 = LINE ( 'NONE', #20196, #19230 ) ;
#4128 = ORIENTED_EDGE ( 'NONE', *, *, #9418, .T. ) ;
#4129 = CARTESIAN_POINT ( 'NONE',  ( -280.8708543776411943, 269.1520027839447948, -146.7592670532759769 ) ) ;
#4130 = VERTEX_POINT ( 'NONE', #21502 ) ;
#4131 = DIRECTION ( 'NONE',  ( -6.580500949201930884E-15, -2.336402151923303105E-15, -1.000000000000000000 ) ) ;
#4132 = EDGE_CURVE ( 'NONE', #4477, #23519, #12032, .T. ) ;
#4133 = CARTESIAN_POINT ( 'NONE',  ( 0.2500000000000002220, 0.000000000000000000, 4.000000000000000000 ) ) ;
#4134 = LINE ( 'NONE', #9362, #11637 ) ;
#4135 = EDGE_CURVE ( 'NONE', #18225, #13331, #10077, .T. ) ;
#4136 = VECTOR ( 'NONE', #13172, 1000.000000000000000 ) ;
#4137 = EDGE_CURVE ( 'NONE', #12774, #8155, #12192, .T. ) ;
#4138 = CARTESIAN_POINT ( 'NONE',  ( 281.9223300543793584, 268.9079617568158938, 145.9952621458756710 ) ) ;
#4139 = CARTESIAN_POINT ( 'NONE',  ( 5.000000000000000000, 3.513898075855358627, -2.028750000000004938 ) ) ;
#4140 = ADVANCED_FACE ( 'NONE', ( #1335 ), #14110, .T. ) ;
#4141 = AXIS2_PLACEMENT_3D ( 'NONE', #10693, #5112, #16452 ) ;
#4142 = VERTEX_POINT ( 'NONE', #23428 ) ;
#4143 = AXIS2_PLACEMENT_3D ( 'NONE', #17218, #4161, #22867 ) ;
#4144 = DIRECTION ( 'NONE',  ( -1.000000000000000000, 0.000000000000000000, 0.000000000000000000 ) ) ;
#4145 = CIRCLE ( 'NONE', #9185, 19.99999999999999645 ) ;
#4146 = EDGE_CURVE ( 'NONE', #18827, #22176, #4845, .T. ) ;
#4147 = FACE_OUTER_BOUND ( 'NONE', #17080, .T. ) ;
#4148 =( REPRESENTATION_RELATIONSHIP ('NONE','NONE', #10127, #5587 ) REPRESENTATION_RELATIONSHIP_WITH_TRANSFORMATION ( #1250 )SHAPE_REPRESENTATION_RELATIONSHIP( ) );
#4149 = EDGE_CURVE ( 'NONE', #21138, #22960, #6894, .T. ) ;
#4150 = LINE ( 'NONE', #22390, #4613 ) ;
#4151 = EDGE_LOOP ( 'NONE', ( #2618, #11876, #12754, #15577 ) ) ;
#4152 = DIRECTION ( 'NONE',  ( 0.000000000000000000, 0.000000000000000000, -1.000000000000000000 ) ) ;
#4153 = EDGE_LOOP ( 'NONE', ( #2818, #16752 ) ) ;
#4154 = LINE ( 'NONE', #22394, #1378 ) ;
#4155 = CARTESIAN_POINT ( 'NONE',  ( -31.74999999999995737, 0.000000000000000000, 0.000000000000000000 ) ) ;
#4156 = EDGE_LOOP ( 'NONE', ( #7443, #19707, #21524, #5570 ) ) ;
#4157 = DIRECTION ( 'NONE',  ( 1.000000000000000000, -0.000000000000000000, 6.982962677686266711E-15 ) ) ;
#4158 = VERTEX_POINT ( 'NONE', #23069 ) ;
#4159 = VECTOR ( 'NONE', #4306, 1000.000000000000000 ) ;
#4160 = CARTESIAN_POINT ( 'NONE',  ( 24.33333333333333215, -89.99999999999998579, 0.000000000000000000 ) ) ;
#4161 = DIRECTION ( 'NONE',  ( -0.000000000000000000, 1.000000000000000000, -0.000000000000000000 ) ) ;
#4162 = DIRECTION ( 'NONE',  ( 1.000000000000000000, 0.000000000000000000, 0.000000000000000000 ) ) ;
#4163 = CARTESIAN_POINT ( 'NONE',  ( 2.000000000000008882, 3.464101615137749945, 0.000000000000000000 ) ) ;
#4164 = AXIS2_PLACEMENT_3D ( 'NONE', #18353, #12621, #17891 ) ;
#4165 = DIRECTION ( 'NONE',  ( -0.000000000000000000, -0.000000000000000000, 1.000000000000000000 ) ) ;
#4166 = AXIS2_PLACEMENT_3D ( 'NONE', #1514, #18396, #9255 ) ;
#4167 = LINE ( 'NONE', #559, #8864 ) ;
#4168 = VECTOR ( 'NONE', #23292, 1000.000000000000000 ) ;
#4169 = CARTESIAN_POINT ( 'NONE',  ( 34.55500000000001393, 0.000000000000000000, 2.500000000000000888 ) ) ;
#4170 = AXIS2_PLACEMENT_3D ( 'NONE', #16262, #5487, #16475 ) ;
#4171 = EDGE_LOOP ( 'NONE', ( #3167, #509 ) ) ;
#4172 = CARTESIAN_POINT ( 'NONE',  ( 80.00000000000001421, -56.79999999999913030, 250.0000000000000000 ) ) ;
#4173 = CARTESIAN_POINT ( 'NONE',  ( 1.567478505476134606E-15, 4.618802153517012066, -5.000000000000000000 ) ) ;
#4174 = EDGE_LOOP ( 'NONE', ( #13858, #6378, #10101, #1243 ) ) ;
#4175 = VERTEX_POINT ( 'NONE', #6779 ) ;
#4176 = DIRECTION ( 'NONE',  ( 1.000000000000000000, 0.000000000000000000, 0.000000000000000000 ) ) ;
#4177 = DIRECTION ( 'NONE',  ( 0.000000000000000000, 0.000000000000000000, 1.000000000000000000 ) ) ;
#4178 = DIRECTION ( 'NONE',  ( 0.000000000000000000, 0.000000000000000000, -1.000000000000000000 ) ) ;
#4179 = CIRCLE ( 'NONE', #6120, 2.649999999999971934 ) ;
#4180 = ORIENTED_EDGE ( 'NONE', *, *, #22954, .F. ) ;
#4181 = EDGE_CURVE ( 'NONE', #21516, #13307, #8239, .T. ) ;
#4182 = AXIS2_PLACEMENT_3D ( 'NONE', #5983, #22872, #20705 ) ;
#4183 = DIRECTION ( 'NONE',  ( -1.000000000000000000, -0.000000000000000000, -0.000000000000000000 ) ) ;
#4184 = EDGE_CURVE ( 'NONE', #10594, #14150, #2506, .T. ) ;
#4185 = FACE_OUTER_BOUND ( 'NONE', #13720, .T. ) ;
#4186 = CIRCLE ( 'NONE', #5345, 2.649999999999971934 ) ;
#4187 = VECTOR ( 'NONE', #3645, 1000.000000000000000 ) ;
#4188 = DIRECTION ( 'NONE',  ( -1.000000000000000000, -0.000000000000000000, -0.000000000000000000 ) ) ;
#4189 = ORIENTED_EDGE ( 'NONE', *, *, #20979, .F. ) ;
#4190 = CYLINDRICAL_SURFACE ( 'NONE', #5602, 2.199999999999979750 ) ;
#4191 = CARTESIAN_POINT ( 'NONE',  ( -288.2000000000008981, 30.00000000000101963, -105.0000000000000142 ) ) ;
#4192 =( NAMED_UNIT ( * ) SI_UNIT ( $, .STERADIAN. ) SOLID_ANGLE_UNIT ( ) );
#4193 = ORIENTED_EDGE ( 'NONE', *, *, #9622, .T. ) ;
#4194 = FACE_OUTER_BOUND ( 'NONE', #13985, .T. ) ;
#4195 = FACE_BOUND ( 'NONE', #9545, .T. ) ;
#4196 = CARTESIAN_POINT ( 'NONE',  ( 99.99999999999987210, -127.0000000000000568, 152.4000000000014268 ) ) ;
#4197 = CARTESIAN_POINT ( 'NONE',  ( -35.00000000000000711, 4.286263797015737285E-15, -100.0000000000000000 ) ) ;
#4198 = ORIENTED_EDGE ( 'NONE', *, *, #18641, .F. ) ;
#4199 = AXIS2_PLACEMENT_3D ( 'NONE', #9108, #10835, #3532 ) ;
#4200 = VERTEX_POINT ( 'NONE', #17636 ) ;
#4201 = AXIS2_PLACEMENT_3D ( 'NONE', #5217, #18484, #20064 ) ;
#4202 = AXIS2_PLACEMENT_3D ( 'NONE', #12311, #15784, #10231 ) ;
#4203 = CARTESIAN_POINT ( 'NONE',  ( 23.72315261474502890, -8.055391459054607850, 145.0000119999999697 ) ) ;
#4204 = CIRCLE ( 'NONE', #18115, 145.0000000000000284 ) ;
#4205 = CARTESIAN_POINT ( 'NONE',  ( 282.2000000000013529, -127.0000000000000568, -146.4928932188134070 ) ) ;
#4206 = CIRCLE ( 'NONE', #21171, 2.649999999999985700 ) ;
#4207 = AXIS2_PLACEMENT_3D ( 'NONE', #4231, #500, #13695 ) ;
#4208 = ORIENTED_EDGE ( 'NONE', *, *, #21744, .T. ) ;
#4209 = DIRECTION ( 'NONE',  ( 1.000000000000000000, 0.000000000000000000, 0.000000000000000000 ) ) ;
#4210 = CARTESIAN_POINT ( 'NONE',  ( 50.00000000000000000, -131.7994082814339833, 3.000000000000000000 ) ) ;
#4211 = AXIS2_PLACEMENT_3D ( 'NONE', #11177, #18722, #15143 ) ;
#4212 = EDGE_LOOP ( 'NONE', ( #7732, #11570, #10090, #10515, #5353 ) ) ;
#4213 = CARTESIAN_POINT ( 'NONE',  ( -25.00000000000001776, 45.00100000000072953, 154.9999999999998579 ) ) ;
#4214 = VERTEX_POINT ( 'NONE', #22946 ) ;
#4216 = AXIS2_PLACEMENT_3D ( 'NONE', #17985, #1431, #16064 ) ;
#4215 = AXIS2_PLACEMENT_3D ( 'NONE', #1841, #3649, #18157 ) ;
#4217 = FACE_OUTER_BOUND ( 'NONE', #8744, .T. ) ;
#4219 = AXIS2_PLACEMENT_3D ( 'NONE', #5605, #13013, #18522 ) ;
#4218 = DIRECTION ( 'NONE',  ( -0.000000000000000000, 1.000000000000000000, 3.495664435217746987E-15 ) ) ;
#4220 = ORIENTED_EDGE ( 'NONE', *, *, #12562, .F. ) ;
#4221 = EDGE_LOOP ( 'NONE', ( #20755, #16672, #22624, #2139 ) ) ;
#4222 = CARTESIAN_POINT ( 'NONE',  ( -100.0000000000000000, 35.00000000000009948, 147.2000000000008413 ) ) ;
#4223 = CIRCLE ( 'NONE', #10430, 2.055000000000001492 ) ;
#4224 = VECTOR ( 'NONE', #11098, 1000.000000000000114 ) ;
#4225 = CARTESIAN_POINT ( 'NONE',  ( 2.500000000000000000, 1.178949249685213863, -2.042000000000001148 ) ) ;
#4226 = AXIS2_PLACEMENT_3D ( 'NONE', #20020, #12709, #7213 ) ;
#4227 = CARTESIAN_POINT ( 'NONE',  ( -64.99999999999998579, -52.79999999999942872, 125.0000000000001421 ) ) ;
#4228 = CARTESIAN_POINT ( 'NONE',  ( 283.4379565153277554, 271.7159870726002850, 145.6846668451111952 ) ) ;
#4229 = CARTESIAN_POINT ( 'NONE',  ( 160.0000000000000000, 1.959434878635765210E-14, -90.00000000000000000 ) ) ;
#4230 = DIRECTION ( 'NONE',  ( 1.000000000000000000, 0.000000000000000000, 0.000000000000000000 ) ) ;
#4231 = CARTESIAN_POINT ( 'NONE',  ( -40.00000000000000000, 100.0000000000000000, 147.2000000000005855 ) ) ;
#4232 = ORIENTED_EDGE ( 'NONE', *, *, #11663, .T. ) ;
#4233 = DIRECTION ( 'NONE',  ( 1.000000000000000000, -0.000000000000000000, -0.000000000000000000 ) ) ;
#4234 = CARTESIAN_POINT ( 'NONE',  ( -146.4450000000000500, -204.4690652294806625, 32.50000000000641620 ) ) ;
#4235 = FILL_AREA_STYLE_COLOUR ( '', #11233 ) ;
#4236 = ORIENTED_EDGE ( 'NONE', *, *, #18741, .F. ) ;
#4238 =( GEOMETRIC_REPRESENTATION_CONTEXT ( 3 ) GLOBAL_UNCERTAINTY_ASSIGNED_CONTEXT ( ( #15507 ) ) GLOBAL_UNIT_ASSIGNED_CONTEXT ( ( #3325, #21804, #14463 ) ) REPRESENTATION_CONTEXT ( 'NONE', 'WORKASPACE' ) );
#4237 = PRODUCT_DEFINITION_FORMATION_WITH_SPECIFIED_SOURCE ( 'ANY', '', #1687, .NOT_KNOWN. ) ;
#4239 = DIRECTION ( 'NONE',  ( -0.000000000000000000, 7.709882115452476934E-17, -1.000000000000000000 ) ) ;
#4240 = CARTESIAN_POINT ( 'NONE',  ( 280.4976310729377929, 269.7223300543794267, -146.1079617568159392 ) ) ;
#4241 = CIRCLE ( 'NONE', #17753, 24.69999999999999929 ) ;
#4242 =( GEOMETRIC_REPRESENTATION_CONTEXT ( 3 ) GLOBAL_UNCERTAINTY_ASSIGNED_CONTEXT ( ( #19091 ) ) GLOBAL_UNIT_ASSIGNED_CONTEXT ( ( #13364, #6428, #22608 ) ) REPRESENTATION_CONTEXT ( 'NONE', 'WORKASPACE' ) );
#4243 = VECTOR ( 'NONE', #12870, 1000.000000000000000 ) ;
#4244 = CIRCLE ( 'NONE', #5411, 2.649999999999985700 ) ;
#4245 = CIRCLE ( 'NONE', #13934, 2.200000000000028155 ) ;
#4246 = VERTEX_POINT ( 'NONE', #1097 ) ;
#4247 = FACE_OUTER_BOUND ( 'NONE', #4678, .T. ) ;
#4248 = ORIENTED_EDGE ( 'NONE', *, *, #3545, .F. ) ;
#4249 = LINE ( 'NONE', #13597, #18307 ) ;
#4250 = CARTESIAN_POINT ( 'NONE',  ( 285.1999999999999318, 267.7999999999999545, -146.4928932188133786 ) ) ;
#4251 = ORIENTED_EDGE ( 'NONE', *, *, #17095, .F. ) ;
#4252 = EDGE_CURVE ( 'NONE', #471, #17932, #18306, .T. ) ;
#4253 = CARTESIAN_POINT ( 'NONE',  ( -280.6220388411723548, 269.5592670532759030, 146.3520027839448119 ) ) ;
#4254 = ADVANCED_FACE ( 'NONE', ( #23197 ), #12254, .T. ) ;
#4255 = EDGE_CURVE ( 'NONE', #18246, #12251, #18233, .T. ) ;
#4256 = CONTEXT_DEPENDENT_SHAPE_REPRESENTATION ( #6180, #7782 ) ;
#4257 = EDGE_LOOP ( 'NONE', ( #11830, #6512, #11286 ) ) ;
#4258 = DIRECTION ( 'NONE',  ( 1.000000000000000000, 0.000000000000000000, 0.000000000000000000 ) ) ;
#4259 = ADVANCED_FACE ( 'NONE', ( #5714 ), #3818, .T. ) ;
#4260 = ORIENTED_EDGE ( 'NONE', *, *, #22259, .F. ) ;
#4261 = FACE_OUTER_BOUND ( 'NONE', #6331, .T. ) ;
#4262 = ADVANCED_FACE ( 'NONE', ( #10789 ), #16213, .F. ) ;
#4263 = LINE ( 'NONE', #20799, #6531 ) ;
#4264 = CIRCLE ( 'NONE', #7355, 2.649999999999971934 ) ;
#4265 = VECTOR ( 'NONE', #3039, 1000.000000000000000 ) ;
#4266 = FACE_BOUND ( 'NONE', #11482, .T. ) ;
#4267 = CARTESIAN_POINT ( 'NONE',  ( -6.473970235329672780E-16, -4.862606272033106691, -3.745885042887442395 ) ) ;
#4268 = VERTEX_POINT ( 'NONE', #16553 ) ;
#4269 = CARTESIAN_POINT ( 'NONE',  ( -282.2000000000000455, 267.7999999999999545, 146.4928932188134354 ) ) ;
#4270 = SURFACE_SIDE_STYLE ('',( #9955 ) ) ;
#4271 = PRODUCT_DEFINITION_SHAPE ( 'NONE', 'NONE',  #23851 ) ;
#4273 = ORIENTED_EDGE ( 'NONE', *, *, #21790, .T. ) ;
#4272 = ORIENTED_EDGE ( 'NONE', *, *, #2812, .F. ) ;
#4274 = DIRECTION ( 'NONE',  ( 0.6964005597823107463, -0.7176533009294141507, 0.000000000000000000 ) ) ;
#4275 = DIRECTION ( 'NONE',  ( -0.000000000000000000, -0.000000000000000000, 1.000000000000000000 ) ) ;
#4276 = LINE ( 'NONE', #11429, #16601 ) ;
#4277 = FACE_OUTER_BOUND ( 'NONE', #12268, .T. ) ;
#4278 = DIRECTION ( 'NONE',  ( -1.000000000000000000, -0.000000000000000000, -0.000000000000000000 ) ) ;
#4279 = ORIENTED_EDGE ( 'NONE', *, *, #18990, .T. ) ;
#4280 = CARTESIAN_POINT ( 'NONE',  ( 0.000000000000000000, 145.0000000000000284, -90.00000000000000000 ) ) ;
#4281 = CARTESIAN_POINT ( 'NONE',  ( 281.4928932188134354, -132.2000000000000455, -177.2000000000013529 ) ) ;
#4282 = CARTESIAN_POINT ( 'NONE',  ( 124.0796955067757494, -1092.893784429268635, 32.42079297023032325 ) ) ;
#4283 = CONTEXT_DEPENDENT_SHAPE_REPRESENTATION ( #4749, #21438 ) ;
#4284 = ORIENTED_EDGE ( 'NONE', *, *, #9177, .T. ) ;
#4285 = CARTESIAN_POINT ( 'NONE',  ( 45.00000000000004974, -59.79999999999964899, 105.0000000000002274 ) ) ;
#4286 = ADVANCED_FACE ( 'NONE', ( #5092 ), #18131, .T. ) ;
#4287 = ORIENTED_EDGE ( 'NONE', *, *, #12558, .F. ) ;
#4288 = DIRECTION ( 'NONE',  ( -1.000000000000000000, 0.000000000000000000, 0.000000000000000000 ) ) ;
#4289 = CARTESIAN_POINT ( 'NONE',  ( -5.384454397937118664, 6.702023979852544604E-16, -5.000000000000000000 ) ) ;
#4290 = ORIENTED_EDGE ( 'NONE', *, *, #2376, .T. ) ;
#4291 = CARTESIAN_POINT ( 'NONE',  ( 12.52393590864757478, 21.69895866456091582, -145.0000000000000000 ) ) ;
#4292 = EDGE_CURVE ( 'NONE', #7788, #14717, #23562, .T. ) ;
#4293 = ORIENTED_EDGE ( 'NONE', *, *, #15282, .F. ) ;
#4294 = CARTESIAN_POINT ( 'NONE',  ( 155.0000000000000284, -500.0000000000000000, -29.99999999999997158 ) ) ;
#4295 = CARTESIAN_POINT ( 'NONE',  ( -0.6448876103708541807, -4.246476118072358474, -0.2256878752776773356 ) ) ;
#4296 = ADVANCED_FACE ( 'NONE', ( #1451 ), #20236, .F. ) ;
#4297 = CYLINDRICAL_SURFACE ( 'NONE', #10029, 2.649999999999999467 ) ;
#4298 = CARTESIAN_POINT ( 'NONE',  ( 0.000000000000000000, 0.000000000000000000, 0.000000000000000000 ) ) ;
#4299 = DIRECTION ( 'NONE',  ( -3.469446951953612710E-16, 1.000000000000000000, 0.000000000000000000 ) ) ;
#4300 = FACE_OUTER_BOUND ( 'NONE', #5, .T. ) ;
#4301 = CARTESIAN_POINT ( 'NONE',  ( -7.500000000000000000, 3.202583086485915942, -7.213046687579523386 ) ) ;
#4302 =( REPRESENTATION_RELATIONSHIP ('NONE','NONE', #10127, #5587 ) REPRESENTATION_RELATIONSHIP_WITH_TRANSFORMATION ( #4515 )SHAPE_REPRESENTATION_RELATIONSHIP( ) );
#4303 = ADVANCED_FACE ( 'NONE', ( #14751 ), #15252, .F. ) ;
#4304 = ORIENTED_EDGE ( 'NONE', *, *, #22470, .T. ) ;
#4305 = EDGE_CURVE ( 'NONE', #9606, #12, #16322, .T. ) ;
#4306 = DIRECTION ( 'NONE',  ( 1.000000000000000000, 3.469446951953614189E-16, 0.000000000000000000 ) ) ;
#4307 = LINE ( 'NONE', #16859, #6183 ) ;
#4308 = VERTEX_POINT ( 'NONE', #1689 ) ;
#4309 = VERTEX_POINT ( 'NONE', #12965 ) ;
#4310 = LINE ( 'NONE', #6244, #6893 ) ;
#4311 = CARTESIAN_POINT ( 'NONE',  ( -49.99999999999997158, -59.80000000000004690, 2.200487334620165724E-13 ) ) ;
#4312 = DIRECTION ( 'NONE',  ( 1.000000000000000000, 0.000000000000000000, 0.000000000000000000 ) ) ;
#4313 = EDGE_LOOP ( 'NONE', ( #23203, #9087, #2978, #2329 ) ) ;
#4314 = PLANE ( 'NONE',  #3005 ) ;
#4315 = FACE_OUTER_BOUND ( 'NONE', #3762, .T. ) ;
#4316 = LINE ( 'NONE', #4433, #20402 ) ;
#4317 = VERTEX_POINT ( 'NONE', #14518 ) ;
#4318 = CARTESIAN_POINT ( 'NONE',  ( 281.2434055557876036, 269.1518577254344677, 150.0327955282141374 ) ) ;
#4319 = DIRECTION ( 'NONE',  ( -1.000000000000000000, -0.000000000000000000, -0.000000000000000000 ) ) ;
#4320 = UNCERTAINTY_MEASURE_WITH_UNIT (LENGTH_MEASURE( 1.000000000000000082E-05 ), #2444, 'distance_accuracy_value', 'NONE');
#4321 = CARTESIAN_POINT ( 'NONE',  ( 17.00000000000000000, 0.000000000000000000, 2.055000000000000160 ) ) ;
#4322 = ORIENTED_EDGE ( 'NONE', *, *, #17266, .T. ) ;
#4323 = CARTESIAN_POINT ( 'NONE',  ( 279.9999999999999432, 269.9696999999999889, -144.9999999999999716 ) ) ;
#4324 = PRODUCT_DEFINITION_SHAPE ( 'NONE', 'NONE',  #23883 ) ;
#4325 = CONTEXT_DEPENDENT_SHAPE_REPRESENTATION ( #9248, #4966 ) ;
#4326 = CARTESIAN_POINT ( 'NONE',  ( -145.0000000000000284, 0.000000000000000000, 90.00000000000000000 ) ) ;
#4327 = DIRECTION ( 'NONE',  ( 0.000000000000000000, 0.000000000000000000, 1.000000000000000000 ) ) ;
#4328 = DIRECTION ( 'NONE',  ( 0.000000000000000000, -0.4999999999999980016, 0.8660254037844397068 ) ) ;
#4329 = ORIENTED_EDGE ( 'NONE', *, *, #18850, .F. ) ;
#4331 = ORIENTED_EDGE ( 'NONE', *, *, #23772, .T. ) ;
#4330 = ADVANCED_FACE ( 'NONE', ( #8836 ), #5318, .T. ) ;
#4332 = EDGE_CURVE ( 'NONE', #20600, #5249, #7129, .T. ) ;
#4333 = CARTESIAN_POINT ( 'NONE',  ( 24.99999999999999289, -1.636246173744675625, 145.0000119999999697 ) ) ;
#4334 = DIRECTION ( 'NONE',  ( 0.8660254037844374864, -0.5000000000000018874, 0.000000000000000000 ) ) ;
#4335 = EDGE_CURVE ( 'NONE', #1398, #4834, #7020, .T. ) ;
#4336 = VERTEX_POINT ( 'NONE', #19812 ) ;
#4337 = DIRECTION ( 'NONE',  ( 3.469446951953614682E-16, -1.000000000000000000, 3.483493295888648978E-15 ) ) ;
#4338 = DIRECTION ( 'NONE',  ( -0.000000000000000000, -0.000000000000000000, 1.000000000000000000 ) ) ;
#4339 = VERTEX_POINT ( 'NONE', #11143 ) ;
#4340 = DIRECTION ( 'NONE',  ( -1.000000000000000000, -0.000000000000000000, -0.000000000000000000 ) ) ;
#4341 = CONICAL_SURFACE ( 'NONE', #22446, 4.171999999999999709, 0.7853981633974613796 ) ;
#4342 = EDGE_LOOP ( 'NONE', ( #14493, #19486, #1002, #23440 ) ) ;
#4343 = DIRECTION ( 'NONE',  ( 1.000000000000000000, -0.000000000000000000, -0.000000000000000000 ) ) ;
#4344 = DIRECTION ( 'NONE',  ( 0.000000000000000000, 0.000000000000000000, 1.000000000000000000 ) ) ;
#4345 = ORIENTED_EDGE ( 'NONE', *, *, #353, .T. ) ;
#4346 = ORIENTED_EDGE ( 'NONE', *, *, #5933, .T. ) ;
#4347 = DIRECTION ( 'NONE',  ( -1.000000000000000000, 0.000000000000000000, -0.000000000000000000 ) ) ;
#4348 = DIRECTION ( 'NONE',  ( 1.000000000000000000, 0.000000000000000000, 0.000000000000000000 ) ) ;
#4349 = DIRECTION ( 'NONE',  ( 1.000000000000000000, 0.000000000000000000, 0.000000000000000000 ) ) ;
#4350 = CARTESIAN_POINT ( 'NONE',  ( 285.2000000000013529, -132.2000000000000455, 146.4928932188134638 ) ) ;
#4351 = PLANE ( 'NONE',  #3428 ) ;
#4352 = ORIENTED_EDGE ( 'NONE', *, *, #3237, .F. ) ;
#4353 = EDGE_CURVE ( 'NONE', #12205, #1524, #12617, .T. ) ;
#4354 = DIRECTION ( 'NONE',  ( -1.000000000000000000, 0.000000000000000000, 0.000000000000000000 ) ) ;
#4355 =( NAMED_UNIT ( * ) PLANE_ANGLE_UNIT ( ) SI_UNIT ( $, .RADIAN. ) );
#4356 = VECTOR ( 'NONE', #13938, 1000.000000000000000 ) ;
#4357 = ORIENTED_EDGE ( 'NONE', *, *, #1235, .F. ) ;
#4358 = EDGE_CURVE ( 'NONE', #949, #10801, #9071, .T. ) ;
#4359 = CARTESIAN_POINT ( 'NONE',  ( 146.4450000000002774, -801.0618695410406644, -32.49999999999356248 ) ) ;
#4360 = DIRECTION ( 'NONE',  ( 0.000000000000000000, -0.4999999999999993894, 0.8660254037844389297 ) ) ;
#4361 = VERTEX_POINT ( 'NONE', #12852 ) ;
#4362 = CARTESIAN_POINT ( 'NONE',  ( -8.050117706004019880, -23.72530153055896207, -145.0000000000000000 ) ) ;
#4363 = ORIENTED_EDGE ( 'NONE', *, *, #12194, .F. ) ;
#4364 = DIRECTION ( 'NONE',  ( -0.000000000000000000, -0.000000000000000000, -1.000000000000000000 ) ) ;
#4365 = DIRECTION ( 'NONE',  ( -0.000000000000000000, -0.000000000000000000, -1.000000000000000000 ) ) ;
#4366 = ORIENTED_EDGE ( 'NONE', *, *, #14229, .T. ) ;
#4367 = VECTOR ( 'NONE', #19599, 1000.000000000000114 ) ;
#4368 = CARTESIAN_POINT ( 'NONE',  ( -280.2488155364689533, 269.9427398886703031, 145.5758453455904373 ) ) ;
#4369 = DIRECTION ( 'NONE',  ( -0.000000000000000000, 0.4999999999999979461, -0.8660254037844397068 ) ) ;
#4370 = ORIENTED_EDGE ( 'NONE', *, *, #8154, .T. ) ;
#4371 = VECTOR ( 'NONE', #87, 1000.000000000000000 ) ;
#4372 = UNCERTAINTY_MEASURE_WITH_UNIT (LENGTH_MEASURE( 1.000000000000000082E-05 ), #12426, 'distance_accuracy_value', 'NONE');
#4373 = CARTESIAN_POINT ( 'NONE',  ( -145.0000000000000284, -5.062647941322544249E-13, -90.00000000000000000 ) ) ;
#4374 = CYLINDRICAL_SURFACE ( 'NONE', #2430, 2.649999999999985700 ) ;
#4375 = CARTESIAN_POINT ( 'NONE',  ( -6.127431526422343306E-17, 9.147862274876549904, -8.047472243342932430 ) ) ;
#4376 = ADVANCED_FACE ( 'NONE', ( #16432 ), #3606, .T. ) ;
#4377 = CYLINDRICAL_SURFACE ( 'NONE', #19990, 2.649999999999971934 ) ;
#4378 = ORIENTED_EDGE ( 'NONE', *, *, #17960, .F. ) ;
#4379 = DIRECTION ( 'NONE',  ( 0.000000000000000000, 0.000000000000000000, 1.000000000000000000 ) ) ;
#4380 = VECTOR ( 'NONE', #17614, 1000.000000000000000 ) ;
#4382 = ORIENTED_EDGE ( 'NONE', *, *, #488, .T. ) ;
#4381 = ORIENTED_EDGE ( 'NONE', *, *, #12291, .T. ) ;
#4383 = VECTOR ( 'NONE', #11332, 1000.000000000000114 ) ;
#4384 = DIRECTION ( 'NONE',  ( -0.9289202219288174023, -0.3702799228849934510, -6.982962677686266711E-15 ) ) ;
#4385 = CARTESIAN_POINT ( 'NONE',  ( -146.0000000000001421, -786.5240652294805841, 30.00000000000641620 ) ) ;
#4386 = CARTESIAN_POINT ( 'NONE',  ( 0.000000000000000000, 0.000000000000000000, 0.000000000000000000 ) ) ;
#4387 = ADVANCED_FACE ( 'NONE', ( #21746 ), #23783, .F. ) ;
#4388 = CARTESIAN_POINT ( 'NONE',  ( 280.2840560642353012, 269.9696999999999889, 145.1244266425810849 ) ) ;
#4389 = CARTESIAN_POINT ( 'NONE',  ( 35.00000000000000711, 0.000000000000000000, -100.0000000000000000 ) ) ;
#4390 = ORIENTED_EDGE ( 'NONE', *, *, #9505, .F. ) ;
#4391 = ADVANCED_FACE ( 'NONE', ( #16673 ), #11025, .F. ) ;
#4392 = CARTESIAN_POINT ( 'NONE',  ( 20.00000000000000000, 0.000000000000000000, -150.0000000000000000 ) ) ;
#4393 = CARTESIAN_POINT ( 'NONE',  ( 2.500000000000000000, -1.178949249685214307, 2.042000000000001592 ) ) ;
#4394 = LINE ( 'NONE', #2344, #13542 ) ;
#4395 = ORIENTED_EDGE ( 'NONE', *, *, #490, .T. ) ;
#4397 = CARTESIAN_POINT ( 'NONE',  ( -49.99999999999997158, -62.00000000000003553, 3.000000000000000000 ) ) ;
#4396 = VECTOR ( 'NONE', #12454, 1000.000000000000000 ) ;
#4398 = EDGE_LOOP ( 'NONE', ( #9314, #14380, #9069, #16829 ) ) ;
#4399 = PLANE ( 'NONE',  #14295 ) ;
#4400 = AXIS2_PLACEMENT_3D ( 'NONE', #6945, #3422, #1375 ) ;
#4401 = DIRECTION ( 'NONE',  ( 1.000000000000000000, 0.000000000000000000, 0.000000000000000000 ) ) ;
#4402 = ORIENTED_EDGE ( 'NONE', *, *, #6799, .T. ) ;
#4403 = CARTESIAN_POINT ( 'NONE',  ( -16.51667796985407932, 18.83873075099288386, -145.0000000000000000 ) ) ;
#4404 = ORIENTED_EDGE ( 'NONE', *, *, #6169, .T. ) ;
#4405 = AXIS2_PLACEMENT_3D ( 'NONE', #10147, #23277, #19405 ) ;
#4406 = CARTESIAN_POINT ( 'NONE',  ( 5.000000000000015099, 0.000000000000000000, 0.000000000000000000 ) ) ;
#4407 = CARTESIAN_POINT ( 'NONE',  ( -1.828356344711647319, -3.563200125723192002, -1.076197711133951296E-14 ) ) ;
#4408 = CARTESIAN_POINT ( 'NONE',  ( 124.5680376182006768, -1092.237904323006887, -27.49999999999351274 ) ) ;
#4409 = CARTESIAN_POINT ( 'NONE',  ( 155.0000000000000284, -210.0000000000003411, -32.49999999999350564 ) ) ;
#4410 = DIRECTION ( 'NONE',  ( 0.000000000000000000, 0.000000000000000000, 1.000000000000000000 ) ) ;
#4411 = DIRECTION ( 'NONE',  ( 0.000000000000000000, 1.000000000000000000, 0.000000000000000000 ) ) ;
#4412 = CARTESIAN_POINT ( 'NONE',  ( 0.000000000000000000, 0.000000000000000000, 0.000000000000000000 ) ) ;
#4413 = MANIFOLD_SOLID_BREP ( 'M5 Clearance Hole2', #2119 ) ;
#4414 = ORIENTED_EDGE ( 'NONE', *, *, #21218, .T. ) ;
#4415 = EDGE_CURVE ( 'NONE', #10471, #2262, #20513, .T. ) ;
#4416 = CIRCLE ( 'NONE', #13715, 7.500000000000000000 ) ;
#4417 = EDGE_CURVE ( 'NONE', #13591, #18466, #22448, .T. ) ;
#4418 = DIRECTION ( 'NONE',  ( 0.000000000000000000, 2.618450529776326854E-15, 1.000000000000000000 ) ) ;
#4419 = CARTESIAN_POINT ( 'NONE',  ( -4.000000000000000000, 1.700094919196744270, -3.320312364301766017 ) ) ;
#4420 = VERTEX_POINT ( 'NONE', #2284 ) ;
#4421 = VERTEX_POINT ( 'NONE', #7599 ) ;
#4422 = VECTOR ( 'NONE', #13159, 999.9999999999998863 ) ;
#4423 = CARTESIAN_POINT ( 'NONE',  ( 25.00000000000001066, 45.00100000000033162, 34.99999999999983658 ) ) ;
#4424 = CARTESIAN_POINT ( 'NONE',  ( 312.2000000000013529, -129.2000000000000455, 146.4928932188134638 ) ) ;
#4425 = EDGE_CURVE ( 'NONE', #21239, #17037, #9682, .T. ) ;
#4426 = CARTESIAN_POINT ( 'NONE',  ( 45.00000000000000000, 272.9999999999999432, 0.000000000000000000 ) ) ;
#4427 = AXIS2_PLACEMENT_3D ( 'NONE', #17887, #21386, #11899 ) ;
#4428 = EDGE_CURVE ( 'NONE', #12251, #3909, #10629, .T. ) ;
#4429 = VECTOR ( 'NONE', #12549, 1000.000000000000000 ) ;
#4430 = CARTESIAN_POINT ( 'NONE',  ( 132.5032837044617793, 80.42329363488335048, 32.42126403526988554 ) ) ;
#4431 = CARTESIAN_POINT ( 'NONE',  ( -122.8605704798721945, 82.74225173005939382, -29.99999999999356604 ) ) ;
#4432 = EDGE_CURVE ( 'NONE', #10931, #5086, #3258, .T. ) ;
#4433 = CARTESIAN_POINT ( 'NONE',  ( -90.00000000000000000, -94.99999999999998579, 3.000000000000000000 ) ) ;
#4434 = ORIENTED_EDGE ( 'NONE', *, *, #12764, .T. ) ;
#4435 = DIRECTION ( 'NONE',  ( 1.000000000000000000, 0.000000000000000000, 0.000000000000000000 ) ) ;
#4436 = CARTESIAN_POINT ( 'NONE',  ( -100.0000000000000284, 5.837466857250891336E-13, 150.2000000000009550 ) ) ;
#4437 = EDGE_CURVE ( 'NONE', #12356, #10574, #23342, .T. ) ;
#4438 = FACE_OUTER_BOUND ( 'NONE', #13083, .T. ) ;
#4439 = ORIENTED_EDGE ( 'NONE', *, *, #22344, .T. ) ;
#4440 = DIRECTION ( 'NONE',  ( 4.183096374613631247E-18, 1.000000000000000000, -0.000000000000000000 ) ) ;
#4442 = AXIS2_PLACEMENT_3D ( 'NONE', #18688, #9678, #7963 ) ;
#4441 = SHAPE_DEFINITION_REPRESENTATION ( #22121, #2341 ) ;
#4443 = DIRECTION ( 'NONE',  ( 0.000000000000000000, 0.000000000000000000, -1.000000000000000000 ) ) ;
#4444 = CARTESIAN_POINT ( 'NONE',  ( -146.0000000000004832, -204.4690652294800657, -27.94499999999356632 ) ) ;
#4445 = DIRECTION ( 'NONE',  ( -1.000000000000000000, 0.000000000000000000, 0.000000000000000000 ) ) ;
#4446 = CIRCLE ( 'NONE', #5608, 5.249999999999949374 ) ;
#4447 = UNCERTAINTY_MEASURE_WITH_UNIT (LENGTH_MEASURE( 1.000000000000000082E-05 ), #9575, 'distance_accuracy_value', 'NONE');
#4448 = ORIENTED_EDGE ( 'NONE', *, *, #16677, .F. ) ;
#4449 = ORIENTED_EDGE ( 'NONE', *, *, #15655, .T. ) ;
#4450 = DIRECTION ( 'NONE',  ( 0.000000000000000000, 0.000000000000000000, -1.000000000000000000 ) ) ;
#4451 = CARTESIAN_POINT ( 'NONE',  ( -4.000000000000000000, -2.309401076758512694, -5.000000000000000000 ) ) ;
#4452 = ORIENTED_EDGE ( 'NONE', *, *, #13396, .F. ) ;
#4453 = EDGE_CURVE ( 'NONE', #2402, #18956, #15645, .T. ) ;
#4454 = VECTOR ( 'NONE', #2143, 1000.000000000000000 ) ;
#4455 = ADVANCED_FACE ( 'NONE', ( #4217 ), #18942, .F. ) ;
#4456 = ORIENTED_EDGE ( 'NONE', *, *, #7402, .F. ) ;
#4457 = CARTESIAN_POINT ( 'NONE',  ( -194.7500000000005116, -494.4690652294794404, -32.49999999999322853 ) ) ;
#4458 = CARTESIAN_POINT ( 'NONE',  ( -65.00000000000000000, -56.79999999999932925, 155.0000000000001705 ) ) ;
#4459 = ORIENTED_EDGE ( 'NONE', *, *, #3574, .T. ) ;
#4460 = EDGE_CURVE ( 'NONE', #18754, #14046, #22163, .T. ) ;
#4461 = FACE_OUTER_BOUND ( 'NONE', #22723, .T. ) ;
#4462 = CIRCLE ( 'NONE', #17187, 2.499999999999998668 ) ;
#4463 = ORIENTED_EDGE ( 'NONE', *, *, #14055, .F. ) ;
#4464 = ADVANCED_FACE ( 'NONE', ( #15349 ), #22685, .T. ) ;
#4465 = ADVANCED_FACE ( 'NONE', ( #2035 ), #7139, .T. ) ;
#4466 = CARTESIAN_POINT ( 'NONE',  ( -4.000000000000000000, -2.309401076758512694, -3.433295621305382461 ) ) ;
#4467 = ADVANCED_FACE ( 'NONE', ( #3962 ), #2152, .F. ) ;
#4468 = DIRECTION ( 'NONE',  ( 0.000000000000000000, -1.000000000000000000, -1.177509268541832635E-16 ) ) ;
#4469 = EDGE_LOOP ( 'NONE', ( #4649, #11714, #18366, #18198 ) ) ;
#4470 = ORIENTED_EDGE ( 'NONE', *, *, #23530, .T. ) ;
#4471 = CARTESIAN_POINT ( 'NONE',  ( 3.540020015735602765, 2.810662092924382627, -3.602146406945867962 ) ) ;
#4472 = PRODUCT_DEFINITION_SHAPE ( 'NONE', 'NONE',  #23872 ) ;
#4473 = DIRECTION ( 'NONE',  ( 3.469446951953614682E-16, -1.000000000000000000, 3.483493295888648978E-15 ) ) ;
#4474 = CARTESIAN_POINT ( 'NONE',  ( 6.601567268551444378, -5.319966374295973743, -7.792327460285856766 ) ) ;
#4475 = CIRCLE ( 'NONE', #19487, 2.199999999999979750 ) ;
#4476 = FACE_OUTER_BOUND ( 'NONE', #23759, .T. ) ;
#4477 = VERTEX_POINT ( 'NONE', #6510 ) ;
#4478 = DIRECTION ( 'NONE',  ( 1.000000000000000000, 0.000000000000000000, 0.000000000000000000 ) ) ;
#4479 = AXIS2_PLACEMENT_3D ( 'NONE', #20915, #2436, #9708 ) ;
#4480 = EDGE_LOOP ( 'NONE', ( #1520, #13055, #2946, #5666 ) ) ;
#4481 = FACE_OUTER_BOUND ( 'NONE', #15999, .T. ) ;
#4482 =( REPRESENTATION_RELATIONSHIP ('NONE','NONE', #10127, #5587 ) REPRESENTATION_RELATIONSHIP_WITH_TRANSFORMATION ( #22477 )SHAPE_REPRESENTATION_RELATIONSHIP( ) );
#4483 = ORIENTED_EDGE ( 'NONE', *, *, #14896, .T. ) ;
#4484 = CARTESIAN_POINT ( 'NONE',  ( 6.487720807569985482, -24.19924082479899852, -145.0000000000000000 ) ) ;
#4485 = ORIENTED_EDGE ( 'NONE', *, *, #9009, .T. ) ;
#4486 = VECTOR ( 'NONE', #2090, 1000.000000000000000 ) ;
#4487 = CARTESIAN_POINT ( 'NONE',  ( -146.4450000000005048, -204.4690652294800088, -27.49999999999356604 ) ) ;
#4488 = CARTESIAN_POINT ( 'NONE',  ( 0.000000000000000000, 0.000000000000000000, 90.00000000000000000 ) ) ;
#4489 = ORIENTED_EDGE ( 'NONE', *, *, #17444, .T. ) ;
#4490 = EDGE_CURVE ( 'NONE', #766, #5818, #11806, .T. ) ;
#4491 = CARTESIAN_POINT ( 'NONE',  ( -281.3684665479256637, 268.0880230824753312, 147.1999999999999886 ) ) ;
#4492 = LINE ( 'NONE', #3019, #4023 ) ;
#4493 = EDGE_CURVE ( 'NONE', #13307, #7122, #13800, .T. ) ;
#4494 = ORIENTED_EDGE ( 'NONE', *, *, #4824, .T. ) ;
#4495 = EDGE_CURVE ( 'NONE', #1277, #5510, #21124, .T. ) ;
#4496 = CARTESIAN_POINT ( 'NONE',  ( 34.75000000000005684, 100.0000000000000000, 145.0000000000000000 ) ) ;
#4497 = CARTESIAN_POINT ( 'NONE',  ( -11.08409875828705893, -977.5314323444980573, -145.0000000000001421 ) ) ;
#4498 = CARTESIAN_POINT ( 'NONE',  ( 2.500000000000000000, 2.357898499370433054, -1.951563910473907981E-15 ) ) ;
#4499 = DIRECTION ( 'NONE',  ( -1.000000000000000000, -0.000000000000000000, -0.000000000000000000 ) ) ;
#4500 = EDGE_LOOP ( 'NONE', ( #14116, #13758, #6776, #2974 ) ) ;
#4501 = DIRECTION ( 'NONE',  ( 0.000000000000000000, 0.000000000000000000, 1.000000000000000000 ) ) ;
#4502 = SURFACE_STYLE_FILL_AREA ( #17191 ) ;
#4503 = DIRECTION ( 'NONE',  ( -1.000000000000000000, -0.000000000000000000, -0.000000000000000000 ) ) ;
#4505 = EDGE_LOOP ( 'NONE', ( #8779, #12804, #18791 ) ) ;
#4504 = ORIENTED_EDGE ( 'NONE', *, *, #2780, .F. ) ;
#4506 = DIRECTION ( 'NONE',  ( -0.9289202219288174023, -0.3702799228849934510, -6.982962677686266711E-15 ) ) ;
#4507 = DIRECTION ( 'NONE',  ( 6.982962677686266711E-15, -9.837870180509810443E-29, 1.000000000000000000 ) ) ;
#4508 = CYLINDRICAL_SURFACE ( 'NONE', #23158, 5.249999999999973355 ) ;
#4509 = DIRECTION ( 'NONE',  ( -0.000000000000000000, 1.000000000000000000, -0.000000000000000000 ) ) ;
#4510 = DIRECTION ( 'NONE',  ( 0.000000000000000000, 0.000000000000000000, 1.000000000000000000 ) ) ;
#4511 = VERTEX_POINT ( 'NONE', #15480 ) ;
#4512 = DIRECTION ( 'NONE',  ( 1.000000000000000000, 0.000000000000000000, 0.000000000000000000 ) ) ;
#4513 = CARTESIAN_POINT ( 'NONE',  ( 102.3500000000000227, -19.99999999999998934, 0.000000000000000000 ) ) ;
#4514 = DIRECTION ( 'NONE',  ( -0.000000000000000000, 1.000000000000000000, 0.000000000000000000 ) ) ;
#4515 = ITEM_DEFINED_TRANSFORMATION ( 'NONE', 'NONE', #15811,  #11210 ) ;
#4516 = VERTEX_POINT ( 'NONE', #12114 ) ;
#4517 = EDGE_CURVE ( 'NONE', #22779, #17746, #947, .T. ) ;
#4518 = DIRECTION ( 'NONE',  ( 0.000000000000000000, -3.495664435217746987E-15, 1.000000000000000000 ) ) ;
#4519 = ORIENTED_EDGE ( 'NONE', *, *, #17042, .F. ) ;
#4520 = DIRECTION ( 'NONE',  ( 0.000000000000000000, 0.5000000000000011102, 0.8660254037844380415 ) ) ;
#4521 = CYLINDRICAL_SURFACE ( 'NONE', #15666, 7.500000000000007105 ) ;
#4522 = ORIENTED_EDGE ( 'NONE', *, *, #8740, .T. ) ;
#4523 = DIRECTION ( 'NONE',  ( 0.000000000000000000, 1.000000000000000000, 0.000000000000000000 ) ) ;
#4524 = EDGE_LOOP ( 'NONE', ( #7154, #12284, #17273, #5472, #3620 ) ) ;
#4525 = CARTESIAN_POINT ( 'NONE',  ( 24.99999999999998224, -1000.000000000000000, 145.0000059999999280 ) ) ;
#4526 = FACE_OUTER_BOUND ( 'NONE', #4469, .T. ) ;
#4527 = DIRECTION ( 'NONE',  ( -0.9510565162951557516, 0.3090169943749406234, 0.000000000000000000 ) ) ;
#4528 = CARTESIAN_POINT ( 'NONE',  ( -146.0000000000004832, -204.4690652294800657, -27.94499999999356632 ) ) ;
#4529 = CARTESIAN_POINT ( 'NONE',  ( -2.804994570502171047, -3.229033611042465335, -3.526374918436838701 ) ) ;
#4530 = AXIS2_PLACEMENT_3D ( 'NONE', #16744, #1755, #12575 ) ;
#4531 = CARTESIAN_POINT ( 'NONE',  ( 1.500000000000000000, 12.00000000000000000, 0.000000000000000000 ) ) ;
#4532 = VERTEX_POINT ( 'NONE', #1201 ) ;
#4533 =( LENGTH_UNIT ( ) NAMED_UNIT ( * ) SI_UNIT ( .MILLI., .METRE. ) );
#4534 = CARTESIAN_POINT ( 'NONE',  ( 70.00000000000000000, -112.6666666666666714, 3.000000000000000000 ) ) ;
#4535 = CIRCLE ( 'NONE', #294, 7.500000000000000000 ) ;
#4536 = LINE ( 'NONE', #22881, #10837 ) ;
#4537 = AXIS2_PLACEMENT_3D ( 'NONE', #1462, #1696, #8851 ) ;
#4538 = VERTEX_POINT ( 'NONE', #23040 ) ;
#4539 = ORIENTED_EDGE ( 'NONE', *, *, #13068, .F. ) ;
#4540 = CIRCLE ( 'NONE', #1446, 2.500000000000000444 ) ;
#4541 = DIRECTION ( 'NONE',  ( 1.000000000000000000, 0.000000000000000000, 0.000000000000000000 ) ) ;
#4542 = FACE_OUTER_BOUND ( 'NONE', #22128, .T. ) ;
#4543 = DIRECTION ( 'NONE',  ( -0.7232617928448825673, 0.6905739489807055653, 6.982962677686266711E-15 ) ) ;
#4544 = CARTESIAN_POINT ( 'NONE',  ( 131.6528213848851294, 81.80793830425585611, 28.88700448195641357 ) ) ;
#4545 = DIRECTION ( 'NONE',  ( -1.000000000000000000, -0.000000000000000000, -0.000000000000000000 ) ) ;
#4546 = CARTESIAN_POINT ( 'NONE',  ( -2.171643655288372443, 3.365003104552320767, 2.541098841762897165E-18 ) ) ;
#4547 = ORIENTED_EDGE ( 'NONE', *, *, #4035, .F. ) ;
#4548 = ADVANCED_FACE ( 'NONE', ( #12357 ), #1067, .T. ) ;
#4549 = CARTESIAN_POINT ( 'NONE',  ( 24.99999999999998224, -1000.000000000000000, -138.9999999999999716 ) ) ;
#4550 = DIRECTION ( 'NONE',  ( 0.000000000000000000, 0.000000000000000000, -1.000000000000000000 ) ) ;
#4551 = CIRCLE ( 'NONE', #11149, 2.055000000000001492 ) ;
#4552 = EDGE_CURVE ( 'NONE', #12588, #21739, #12230, .T. ) ;
#4553 = FACE_BOUND ( 'NONE', #10381, .T. ) ;
#4554 = ADVANCED_FACE ( 'NONE', ( #2642 ), #15941, .F. ) ;
#4555 = CIRCLE ( 'NONE', #14221, 2.649999999999985700 ) ;
#4556 = ORIENTED_EDGE ( 'NONE', *, *, #288, .F. ) ;
#4557 = CYLINDRICAL_SURFACE ( 'NONE', #2306, 2.500000000000002220 ) ;
#4558 = CIRCLE ( 'NONE', #3385, 7.500000000000002665 ) ;
#4559 = CONTEXT_DEPENDENT_SHAPE_REPRESENTATION ( #21584, #15965 ) ;
#4560 = FACE_OUTER_BOUND ( 'NONE', #13739, .T. ) ;
#4561 = ADVANCED_FACE ( 'NONE', ( #2869, #21359 ), #10047, .T. ) ;
#4562 = CARTESIAN_POINT ( 'NONE',  ( 2.500000000000000000, -1.178949249685213863, 2.042000000000002924 ) ) ;
#4563 = CARTESIAN_POINT ( 'NONE',  ( 7.499999999999999112, 0.000000000000000000, -100.0000000000000000 ) ) ;
#4564 = ORIENTED_EDGE ( 'NONE', *, *, #5166, .T. ) ;
#4565 = EDGE_LOOP ( 'NONE', ( #9116, #9718 ) ) ;
#4566 = CARTESIAN_POINT ( 'NONE',  ( -44.99999999999997868, -56.79999999999936477, 195.0000000000001705 ) ) ;
#4567 = CARTESIAN_POINT ( 'NONE',  ( -130.4031948627971076, -44.80746418436799416, -90.00000000000000000 ) ) ;
#4568 = ORIENTED_EDGE ( 'NONE', *, *, #6949, .T. ) ;
#4569 = EDGE_CURVE ( 'NONE', #21305, #13461, #20628, .T. ) ;
#4570 = AXIS2_PLACEMENT_3D ( 'NONE', #8965, #7134, #1342 ) ;
#4571 = AXIS2_PLACEMENT_3D ( 'NONE', #1784, #229, #9662 ) ;
#4572 = ORIENTED_EDGE ( 'NONE', *, *, #14395, .T. ) ;
#4573 = CARTESIAN_POINT ( 'NONE',  ( 280.9952621458755289, 270.4339272673396977, 149.5699028110927884 ) ) ;
#4574 = CIRCLE ( 'NONE', #725, 23.97500000000000497 ) ;
#4575 = DIRECTION ( 'NONE',  ( -0.000000000000000000, -0.000000000000000000, -1.000000000000000000 ) ) ;
#4576 = ORIENTED_EDGE ( 'NONE', *, *, #20520, .T. ) ;
#4577 = DIRECTION ( 'NONE',  ( 0.000000000000000000, 0.000000000000000000, -1.000000000000000000 ) ) ;
#4578 = CIRCLE ( 'NONE', #22300, 4.250000000000000000 ) ;
#4579 = ORIENTED_EDGE ( 'NONE', *, *, #2382, .F. ) ;
#4580 = CARTESIAN_POINT ( 'NONE',  ( 155.0000000000000284, -500.0000000000000000, 30.00000000000001421 ) ) ;
#4581 = DIRECTION ( 'NONE',  ( 0.000000000000000000, -0.000000000000000000, 1.000000000000000000 ) ) ;
#4582 = ORIENTED_EDGE ( 'NONE', *, *, #12252, .F. ) ;
#4583 = ORIENTED_EDGE ( 'NONE', *, *, #3539, .F. ) ;
#4584 = DIRECTION ( 'NONE',  ( 3.736327486719275871E-16, -1.000000000000000000, 3.469446951953613794E-15 ) ) ;
#4585 = DIRECTION ( 'NONE',  ( -0.000000000000000000, -0.000000000000000000, 1.000000000000000000 ) ) ;
#4587 = VECTOR ( 'NONE', #5751, 1000.000000000000000 ) ;
#4586 = PRESENTATION_LAYER_ASSIGNMENT (  '', '', ( #13111 ) ) ;
#4588 = VECTOR ( 'NONE', #14718, 1000.000000000000000 ) ;
#4589 = EDGE_CURVE ( 'NONE', #21635, #20633, #2117, .T. ) ;
#4590 = AXIS2_PLACEMENT_3D ( 'NONE', #21590, #6848, #21810 ) ;
#4591 = DIRECTION ( 'NONE',  ( -0.000000000000000000, 0.000000000000000000, -1.000000000000000000 ) ) ;
#4592 = AXIS2_PLACEMENT_3D ( 'NONE', #23691, #18371, #10935 ) ;
#4593 = AXIS2_PLACEMENT_3D ( 'NONE', #7980, #22700, #13330 ) ;
#4594 = EDGE_CURVE ( 'NONE', #3058, #19747, #6279, .T. ) ;
#4595 = VERTEX_POINT ( 'NONE', #23171 ) ;
#4596 = EDGE_CURVE ( 'NONE', #8654, #13423, #4446, .T. ) ;
#4597 = CARTESIAN_POINT ( 'NONE',  ( 60.00000000000000000, -59.79999999999974847, 74.99940828143404303 ) ) ;
#4598 = CIRCLE ( 'NONE', #363, 2.055000000000000160 ) ;
#4599 = EDGE_CURVE ( 'NONE', #3749, #16162, #6439, .T. ) ;
#4600 = ORIENTED_EDGE ( 'NONE', *, *, #9120, .T. ) ;
#4601 = PRODUCT_DEFINITION ( 'UNKNOWN', '', #19285, #5664 ) ;
#4602 = EDGE_CURVE ( 'NONE', #1617, #301, #11872, .T. ) ;
#4603 = VERTEX_POINT ( 'NONE', #22920 ) ;
#4604 = VECTOR ( 'NONE', #22600, 1000.000000000000114 ) ;
#4605 = LINE ( 'NONE', #6411, #8756 ) ;
#4606 = AXIS2_PLACEMENT_3D ( 'NONE', #1248, #7269, #21877 ) ;
#4607 = PRESENTATION_LAYER_ASSIGNMENT (  '', '', ( #6534 ) ) ;
#4608 = EDGE_LOOP ( 'NONE', ( #20905, #572, #9873, #15232 ) ) ;
#4609 = VECTOR ( 'NONE', #11699, 1000.000000000000000 ) ;
#4610 = LINE ( 'NONE', #23061, #7943 ) ;
#4611 = CIRCLE ( 'NONE', #10812, 2.649999999999971934 ) ;
#4612 = DIRECTION ( 'NONE',  ( 0.000000000000000000, -1.000000000000000000, 1.287488025362403787E-15 ) ) ;
#4613 = VECTOR ( 'NONE', #4514, 1000.000000000000000 ) ;
#4614 = ORIENTED_EDGE ( 'NONE', *, *, #7106, .T. ) ;
#4615 = CARTESIAN_POINT ( 'NONE',  ( -280.8708543776413080, 271.0140793454687582, 149.1822575857424624 ) ) ;
#4616 = DIRECTION ( 'NONE',  ( 6.753181414994864868E-15, 0.000000000000000000, -1.000000000000000000 ) ) ;
#4617 = ORIENTED_EDGE ( 'NONE', *, *, #23070, .F. ) ;
#4618 = DIRECTION ( 'NONE',  ( 0.9289202219288174023, 0.3702799228849934510, 6.982962677686266711E-15 ) ) ;
#4619 = CARTESIAN_POINT ( 'NONE',  ( -24.99999999999996092, -37.41657386773943728, 35.00000000000013500 ) ) ;
#4620 = CARTESIAN_POINT ( 'NONE',  ( 5.000000000000000000, 2.342598717236902939, -4.057500000000001883 ) ) ;
#4621 = CARTESIAN_POINT ( 'NONE',  ( 89.00000000000000000, -74.99999999999998579, 3.000000000000000000 ) ) ;
#4622 = ORIENTED_EDGE ( 'NONE', *, *, #7945, .F. ) ;
#4624 = VECTOR ( 'NONE', #19907, 1000.000000000000114 ) ;
#4623 = MECHANICAL_DESIGN_GEOMETRIC_PRESENTATION_REPRESENTATION (  '', ( #6554 ), #18861 ) ;
#4625 = FACE_OUTER_BOUND ( 'NONE', #6996, .T. ) ;
#4626 = FILL_AREA_STYLE_COLOUR ( '', #8104 ) ;
#4627 = MECHANICAL_DESIGN_GEOMETRIC_PRESENTATION_REPRESENTATION (  '', ( #1161 ), #13538 ) ;
#4628 = CIRCLE ( 'NONE', #5409, 5.199999999999982414 ) ;
#4629 = CIRCLE ( 'NONE', #14678, 20.00000000000000000 ) ;
#4630 = VECTOR ( 'NONE', #14586, 1000.000000000000000 ) ;
#4632 = ORIENTED_EDGE ( 'NONE', *, *, #13014, .F. ) ;
#4631 = ORIENTED_EDGE ( 'NONE', *, *, #1244, .T. ) ;
#4633 = DIRECTION ( 'NONE',  ( 6.982962677686266711E-15, 0.000000000000000000, -1.000000000000000000 ) ) ;
#4634 = EDGE_CURVE ( 'NONE', #327, #7954, #837, .T. ) ;
#4635 = EDGE_CURVE ( 'NONE', #23122, #5697, #22266, .T. ) ;
#4636 = CARTESIAN_POINT ( 'NONE',  ( 7.922811941611899833, 4.628808333142401032, -8.057670691780701944 ) ) ;
#4637 = CARTESIAN_POINT ( 'NONE',  ( -121.5574576620393970, -79.04925354955290118, -2.775557561562891351E-14 ) ) ;
#4638 = EDGE_CURVE ( 'NONE', #13229, #14636, #20254, .T. ) ;
#4639 = VECTOR ( 'NONE', #12672, 1000.000000000000000 ) ;
#4640 = DIRECTION ( 'NONE',  ( -0.000000000000000000, -0.000000000000000000, -1.000000000000000000 ) ) ;
#4641 = CARTESIAN_POINT ( 'NONE',  ( 5.000000000000000000, 0.000000000000000000, 0.000000000000000000 ) ) ;
#4642 = CARTESIAN_POINT ( 'NONE',  ( -284.5436892194422285, 270.4188186979286002, -145.9952621458756141 ) ) ;
#4643 = VERTEX_POINT ( 'NONE', #16182 ) ;
#4644 = CARTESIAN_POINT ( 'NONE',  ( 25.00000000000000000, -1.196402736354634486E-15, -145.0000119999999697 ) ) ;
#4645 = AXIS2_PLACEMENT_3D ( 'NONE', #14277, #9053, #17866 ) ;
#4646 = CARTESIAN_POINT ( 'NONE',  ( 0.000000000000000000, 0.000000000000000000, -100.0000000000000000 ) ) ;
#4647 = LINE ( 'NONE', #4876, #1521 ) ;
#4648 = AXIS2_PLACEMENT_3D ( 'NONE', #19889, #23398, #3341 ) ;
#4649 = ORIENTED_EDGE ( 'NONE', *, *, #1934, .F. ) ;
#4650 = AXIS2_PLACEMENT_3D ( 'NONE', #228, #13301, #6137 ) ;
#4651 = LINE ( 'NONE', #9853, #5144 ) ;
#4652 = EDGE_LOOP ( 'NONE', ( #11629, #14445, #22052, #17757 ) ) ;
#4653 = CARTESIAN_POINT ( 'NONE',  ( -7.500000000000000000, 4.330127018922191873, -10.00000000000000000 ) ) ;
#4654 = CARTESIAN_POINT ( 'NONE',  ( 281.4928932188134354, 5.173457871231059415E-13, -150.2000000000008981 ) ) ;
#4655 = ORIENTED_EDGE ( 'NONE', *, *, #21263, .T. ) ;
#4656 = CARTESIAN_POINT ( 'NONE',  ( 1.642023387316846605, 25.00004926070564082, -145.0000000000000000 ) ) ;
#4657 = ORIENTED_EDGE ( 'NONE', *, *, #3373, .F. ) ;
#4658 =( NAMED_UNIT ( * ) SI_UNIT ( $, .STERADIAN. ) SOLID_ANGLE_UNIT ( ) );
#4659 = CARTESIAN_POINT ( 'NONE',  ( -7.922281120364393914, 4.573931137438271399, -8.047472243342930653 ) ) ;
#4660 = DIRECTION ( 'NONE',  ( 1.000000000000000000, 0.000000000000000000, 0.000000000000000000 ) ) ;
#4661 = DIRECTION ( 'NONE',  ( 1.000000000000000000, 0.000000000000000000, 0.000000000000000000 ) ) ;
#4662 = CYLINDRICAL_SURFACE ( 'NONE', #11988, 2.199999999999979750 ) ;
#4663 = DIRECTION ( 'NONE',  ( -0.000000000000000000, 0.000000000000000000, -1.000000000000000000 ) ) ;
#4664 = MANIFOLD_SOLID_BREP ( 'Hex', #18690 ) ;
#4665 = ORIENTED_EDGE ( 'NONE', *, *, #5661, .F. ) ;
#4666 = EDGE_LOOP ( 'NONE', ( #18130, #15538, #11354, #22381 ) ) ;
#4667 = DIRECTION ( 'NONE',  ( 0.000000000000000000, 0.000000000000000000, -1.000000000000000000 ) ) ;
#4668 = CARTESIAN_POINT ( 'NONE',  ( -4.000000000000000000, 2.511478553582031203, -3.469254451724764543 ) ) ;
#4669 = ORIENTED_EDGE ( 'NONE', *, *, #14313, .F. ) ;
#4670 = ORIENTED_EDGE ( 'NONE', *, *, #4721, .F. ) ;
#4671 = CARTESIAN_POINT ( 'NONE',  ( 67.35000000000002274, -87.33333333333332860, 0.000000000000000000 ) ) ;
#4672 = CARTESIAN_POINT ( 'NONE',  ( 0.000000000000000000, 0.000000000000000000, 124.9999999999999716 ) ) ;
#4674 = FACE_OUTER_BOUND ( 'NONE', #16028, .T. ) ;
#4673 = PRODUCT_DEFINITION_SHAPE ( 'NONE', 'NONE',  #23878 ) ;
#4675 = CARTESIAN_POINT ( 'NONE',  ( 100.0000000000000000, 0.000000000000000000, 0.000000000000000000 ) ) ;
#4676 = DIRECTION ( 'NONE',  ( 0.000000000000000000, 0.000000000000000000, 1.000000000000000000 ) ) ;
#4677 = DIRECTION ( 'NONE',  ( 0.000000000000000000, 1.177509268541832635E-16, -1.000000000000000000 ) ) ;
#4678 = EDGE_LOOP ( 'NONE', ( #15846, #11720, #3653, #7925 ) ) ;
#4679 = DIRECTION ( 'NONE',  ( 0.000000000000000000, 0.000000000000000000, -1.000000000000000000 ) ) ;
#4680 = DIRECTION ( 'NONE',  ( 0.000000000000000000, -0.000000000000000000, 1.000000000000000000 ) ) ;
#4681 = CARTESIAN_POINT ( 'NONE',  ( -146.0000000000000853, -494.4690652294807478, 30.00000000000641620 ) ) ;
#4682 = ORIENTED_EDGE ( 'NONE', *, *, #12724, .T. ) ;
#4683 = LINE ( 'NONE', #13900, #23065 ) ;
#4684 = SHAPE_REPRESENTATION ( 'belt', ( #11210 ), #5408 ) ;
#4685 = CARTESIAN_POINT ( 'NONE',  ( -140.0355749532211007, 37.61698748598567477, 90.00000000000000000 ) ) ;
#4686 = CARTESIAN_POINT ( 'NONE',  ( -22.46856765566313996, -1011.084098757902211, -145.0000000000001421 ) ) ;
#4687 = DIRECTION ( 'NONE',  ( 0.000000000000000000, 0.000000000000000000, 1.000000000000000000 ) ) ;
#4688 = EDGE_CURVE ( 'NONE', #748, #4158, #13158, .T. ) ;
#4689 = CARTESIAN_POINT ( 'NONE',  ( -155.0000000000000284, -784.4690652294804067, 30.00000000000648015 ) ) ;
#4690 = ORIENTED_EDGE ( 'NONE', *, *, #7220, .F. ) ;
#4691 = VERTEX_POINT ( 'NONE', #18634 ) ;
#4692 = DIRECTION ( 'NONE',  ( 0.000000000000000000, 1.000000000000000000, 0.000000000000000000 ) ) ;
#4693 = CARTESIAN_POINT ( 'NONE',  ( -7.640563834021360018E-16, -9.147862274876560562, -8.047472243342937759 ) ) ;
#4694 = ORIENTED_EDGE ( 'NONE', *, *, #11717, .T. ) ;
#4695 = EDGE_CURVE ( 'NONE', #7126, #6295, #10256, .T. ) ;
#4696 = EDGE_CURVE ( 'NONE', #2692, #17768, #6869, .T. ) ;
#4697 = ORIENTED_EDGE ( 'NONE', *, *, #577, .T. ) ;
#4698 = CARTESIAN_POINT ( 'NONE',  ( -44.99999999999995026, -56.79999999999967741, 107.6500000000002188 ) ) ;
#4699 = LINE ( 'NONE', #9784, #21101 ) ;
#4700 = ORIENTED_EDGE ( 'NONE', *, *, #17868, .T. ) ;
#4701 = CARTESIAN_POINT ( 'NONE',  ( -135.3962747006864618, -1075.451122483741301, -27.62619522811935013 ) ) ;
#4702 = ADVANCED_FACE ( 'NONE', ( #14933, #2099, #9493, #3230, #20574 ), #16845, .T. ) ;
#4703 = VERTEX_POINT ( 'NONE', #1426 ) ;
#4704 = DIRECTION ( 'NONE',  ( 0.000000000000000000, 1.000000000000000000, 0.000000000000000000 ) ) ;
#4705 = CARTESIAN_POINT ( 'NONE',  ( -7.907996613752304782, -3.055722423191990611, -7.792112796859422374 ) ) ;
#4706 = VERTEX_POINT ( 'NONE', #14817 ) ;
#4707 = VERTEX_POINT ( 'NONE', #21722 ) ;
#4708 = CARTESIAN_POINT ( 'NONE',  ( 133.4862419878495814, 78.78097527456746718, -32.17346063704739834 ) ) ;
#4709 = CARTESIAN_POINT ( 'NONE',  ( 2.725741868436127202, -3.045094352033990148, -3.220599429844051453 ) ) ;
#4710 = DIRECTION ( 'NONE',  ( -1.000000000000000000, -0.000000000000000000, -0.000000000000000000 ) ) ;
#4711 = LINE ( 'NONE', #17765, #2419 ) ;
#4712 = ORIENTED_EDGE ( 'NONE', *, *, #13940, .T. ) ;
#4713 = CARTESIAN_POINT ( 'NONE',  ( -64.99999999999995737, -52.79999999999965610, 65.00000000000017053 ) ) ;
#4714 =( LENGTH_UNIT ( ) NAMED_UNIT ( * ) SI_UNIT ( .MILLI., .METRE. ) );
#4715 = ORIENTED_EDGE ( 'NONE', *, *, #2337, .T. ) ;
#4716 = VECTOR ( 'NONE', #18702, 1000.000000000000000 ) ;
#4717 = ORIENTED_EDGE ( 'NONE', *, *, #3992, .T. ) ;
#4718 = DIRECTION ( 'NONE',  ( 0.000000000000000000, -0.4999999999999991118, 0.8660254037844391517 ) ) ;
#4719 = ORIENTED_EDGE ( 'NONE', *, *, #3453, .T. ) ;
#4720 = LINE ( 'NONE', #16207, #191 ) ;
#4721 = EDGE_CURVE ( 'NONE', #21286, #17297, #14272, .T. ) ;
#4722 = CARTESIAN_POINT ( 'NONE',  ( 0.000000000000000000, 1.178949249685212086, -2.042000000000002036 ) ) ;
#4723 = EDGE_CURVE ( 'NONE', #19341, #22268, #10649, .T. ) ;
#4724 = EDGE_LOOP ( 'NONE', ( #16323, #23364, #21725 ) ) ;
#4725 = LINE ( 'NONE', #10076, #7330 ) ;
#4726 = CARTESIAN_POINT ( 'NONE',  ( -194.7500000000000000, -784.4690652294799520, 32.50000000000675726 ) ) ;
#4727 = ORIENTED_EDGE ( 'NONE', *, *, #5550, .F. ) ;
#4728 = EDGE_CURVE ( 'NONE', #3347, #21577, #13357, .T. ) ;
#4729 = DIRECTION ( 'NONE',  ( 1.110223024625155594E-14, 0.000000000000000000, -1.000000000000000000 ) ) ;
#4730 = SURFACE_SIDE_STYLE ('',( #18011 ) ) ;
#4731 = ADVANCED_FACE ( 'NONE', ( #23541 ), #18105, .F. ) ;
#4732 = DIRECTION ( 'NONE',  ( 0.000000000000000000, 1.000000000000000000, -5.286776307738891306E-15 ) ) ;
#4733 = AXIS2_PLACEMENT_3D ( 'NONE', #20500, #3948, #2138 ) ;
#4734 = DIRECTION ( 'NONE',  ( 0.000000000000000000, 0.000000000000000000, -1.000000000000000000 ) ) ;
#4735 = ORIENTED_EDGE ( 'NONE', *, *, #1244, .F. ) ;
#4736 = CARTESIAN_POINT ( 'NONE',  ( 1.970645868709624460E-14, -56.79999999999915872, 250.0000000000000000 ) ) ;
#4737 = ITEM_DEFINED_TRANSFORMATION ( 'NONE', 'NONE', #21213,  #11210 ) ;
#4739 = ORIENTED_EDGE ( 'NONE', *, *, #11255, .F. ) ;
#4738 = ORIENTED_EDGE ( 'NONE', *, *, #21408, .F. ) ;
#4740 = CARTESIAN_POINT ( 'NONE',  ( 45.00000000000002842, -64.79999999999935767, 340.0000000000002274 ) ) ;
#4741 = FACE_OUTER_BOUND ( 'NONE', #4821, .T. ) ;
#4742 = CARTESIAN_POINT ( 'NONE',  ( 126.7787238282395208, 77.44864885511604768, 27.50000000000641975 ) ) ;
#4743 = FACE_OUTER_BOUND ( 'NONE', #20923, .T. ) ;
#4744 = DIRECTION ( 'NONE',  ( -1.000000000000000000, 0.000000000000000000, 0.000000000000000000 ) ) ;
#4745 = CARTESIAN_POINT ( 'NONE',  ( -280.2880230824754335, 269.9999999999999432, -145.1244266708878570 ) ) ;
#4746 = EDGE_CURVE ( 'NONE', #2501, #16285, #3272, .T. ) ;
#4747 = EDGE_LOOP ( 'NONE', ( #3387, #11767, #11004, #1824, #16928 ) ) ;
#4748 = CONICAL_SURFACE ( 'NONE', #18238, 2.055000000000001492, 0.7853981633974633780 ) ;
#4749 =( REPRESENTATION_RELATIONSHIP ('NONE','NONE', #10127, #18083 ) REPRESENTATION_RELATIONSHIP_WITH_TRANSFORMATION ( #18751 )SHAPE_REPRESENTATION_RELATIONSHIP( ) );
#4750 = LINE ( 'NONE', #19586, #22253 ) ;
#4751 = ORIENTED_EDGE ( 'NONE', *, *, #16662, .F. ) ;
#4752 = CARTESIAN_POINT ( 'NONE',  ( -137.9031948627971076, -44.80746418436799416, 90.00000000000000000 ) ) ;
#4753 = DIRECTION ( 'NONE',  ( -0.000000000000000000, -0.000000000000000000, -1.000000000000000000 ) ) ;
#4754 = VERTEX_POINT ( 'NONE', #9611 ) ;
#4755 = LINE ( 'NONE', #7374, #3967 ) ;
#4756 = ORIENTED_EDGE ( 'NONE', *, *, #13639, .T. ) ;
#4757 = LINE ( 'NONE', #13742, #8881 ) ;
#4758 = DIRECTION ( 'NONE',  ( 6.753181414994864868E-15, 0.000000000000000000, -1.000000000000000000 ) ) ;
#4759 = EDGE_CURVE ( 'NONE', #5473, #13664, #21188, .T. ) ;
#4760 = VERTEX_POINT ( 'NONE', #18888 ) ;
#4761 = EDGE_CURVE ( 'NONE', #15959, #10287, #786, .T. ) ;
#4762 = CARTESIAN_POINT ( 'NONE',  ( 23.72540896990116721, 8.050072860352383231, -145.0000000000000000 ) ) ;
#4763 = DIRECTION ( 'NONE',  ( 1.000000000000000000, 0.000000000000000000, 0.000000000000000000 ) ) ;
#4764 = FACE_OUTER_BOUND ( 'NONE', #20383, .T. ) ;
#4765 = CIRCLE ( 'NONE', #14812, 2.500000000000000444 ) ;
#4766 = PRODUCT ( 'head cover', 'head cover', '', ( #5785 ) ) ;
#4767 = AXIS2_PLACEMENT_3D ( 'NONE', #6937, #10335, #17811 ) ;
#4768 = DIRECTION ( 'NONE',  ( 0.000000000000000000, 0.000000000000000000, 1.000000000000000000 ) ) ;
#4769 = CARTESIAN_POINT ( 'NONE',  ( 280.1452901038202299, 270.0000000000000000, 145.0627656775837124 ) ) ;
#4770 = DIRECTION ( 'NONE',  ( -1.350636282998972974E-14, 0.000000000000000000, -1.000000000000000000 ) ) ;
#4771 = FACE_BOUND ( 'NONE', #1562, .T. ) ;
#4772 = ORIENTED_EDGE ( 'NONE', *, *, #10521, .T. ) ;
#4773 = SURFACE_STYLE_USAGE ( .BOTH. , #1384 ) ;
#4774 = CARTESIAN_POINT ( 'NONE',  ( 21.00000000000000355, 0.000000000000000000, 2.055000000000000160 ) ) ;
#4775 = CARTESIAN_POINT ( 'NONE',  ( 7.500000000000000000, 4.330127018922190096, -10.00000000000000000 ) ) ;
#4776 = ORIENTED_EDGE ( 'NONE', *, *, #2389, .F. ) ;
#4777 = ORIENTED_EDGE ( 'NONE', *, *, #7211, .F. ) ;
#4778 = LINE ( 'NONE', #3081, #18840 ) ;
#4779 = DIRECTION ( 'NONE',  ( 1.000000000000000000, 0.000000000000000000, 0.000000000000000000 ) ) ;
#4780 = DIRECTION ( 'NONE',  ( -1.000000000000000000, -0.000000000000000000, -0.000000000000000000 ) ) ;
#4781 = MECHANICAL_DESIGN_GEOMETRIC_PRESENTATION_REPRESENTATION (  '', ( #15609 ), #3602 ) ;
#4782 = EDGE_CURVE ( 'NONE', #6740, #13908, #2884, .T. ) ;
#4783 = AXIS2_PLACEMENT_3D ( 'NONE', #23387, #3103, #14247 ) ;
#4784 = CARTESIAN_POINT ( 'NONE',  ( 131.5858269427383505, 81.91565353609590261, 30.81384172145501665 ) ) ;
#4785 = DIRECTION ( 'NONE',  ( 0.000000000000000000, 1.000000000000000000, 0.000000000000000000 ) ) ;
#4786 = CARTESIAN_POINT ( 'NONE',  ( -7.499999999999999112, 0.000000000000000000, -100.0000000000000000 ) ) ;
#4787 = ORIENTED_EDGE ( 'NONE', *, *, #2304, .T. ) ;
#4788 = CARTESIAN_POINT ( 'NONE',  ( 45.00000000000004974, -56.79999999999966320, 52.65000000000019753 ) ) ;
#4789 = CARTESIAN_POINT ( 'NONE',  ( 90.00000000000000000, -74.99999999999998579, 0.000000000000000000 ) ) ;
#4790 = ADVANCED_FACE ( 'NONE', ( #17337 ), #4521, .F. ) ;
#4791 = CARTESIAN_POINT ( 'NONE',  ( 100.0000000000000000, -1400.000000000000000, -125.0000000000001705 ) ) ;
#4792 = ORIENTED_EDGE ( 'NONE', *, *, #18293, .F. ) ;
#4793 = FILL_AREA_STYLE ('',( #21336 ) ) ;
#4794 = PLANE ( 'NONE',  #22645 ) ;
#4795 = EDGE_CURVE ( 'NONE', #22159, #12385, #17089, .T. ) ;
#4796 = CYLINDRICAL_SURFACE ( 'NONE', #11636, 2.500000000000002220 ) ;
#4797 = DIRECTION ( 'NONE',  ( -1.000000000000000000, -3.469446951953630952E-16, -4.625929269271472109E-16 ) ) ;
#4798 = CARTESIAN_POINT ( 'NONE',  ( -59.99999999999996447, -136.2780879378741474, -5.721320343559392896 ) ) ;
#4799 = FACE_OUTER_BOUND ( 'NONE', #17556, .T. ) ;
#4800 = DIRECTION ( 'NONE',  ( 1.000000000000000000, 0.000000000000000000, -0.000000000000000000 ) ) ;
#4801 = VECTOR ( 'NONE', #3914, 1000.000000000000000 ) ;
#4802 = ORIENTED_EDGE ( 'NONE', *, *, #11282, .T. ) ;
#4803 = AXIS2_PLACEMENT_3D ( 'NONE', #3179, #23705, #19729 ) ;
#4804 = ORIENTED_EDGE ( 'NONE', *, *, #19808, .T. ) ;
#4805 = LINE ( 'NONE', #23022, #21873 ) ;
#4806 = DIRECTION ( 'NONE',  ( -0.000000000000000000, 0.000000000000000000, -1.000000000000000000 ) ) ;
#4807 = ORIENTED_EDGE ( 'NONE', *, *, #18145, .F. ) ;
#4808 = VECTOR ( 'NONE', #9757, 1000.000000000000114 ) ;
#4809 = FACE_OUTER_BOUND ( 'NONE', #7971, .T. ) ;
#4810 = ORIENTED_EDGE ( 'NONE', *, *, #22437, .F. ) ;
#4811 = FACE_OUTER_BOUND ( 'NONE', #22863, .T. ) ;
#4812 = CARTESIAN_POINT ( 'NONE',  ( -126.8186628169060981, 89.11812652456482908, 28.34183984639740572 ) ) ;
#4813 = ORIENTED_EDGE ( 'NONE', *, *, #14907, .F. ) ;
#4814 = CARTESIAN_POINT ( 'NONE',  ( -134.5479913728703991, -1076.953479568426019, -30.32849798811268727 ) ) ;
#4815 = SHAPE_REPRESENTATION ( 'bucket', ( #11210 ), #1906 ) ;
#4816 = ORIENTED_EDGE ( 'NONE', *, *, #320, .T. ) ;
#4817 = B_SPLINE_CURVE_WITH_KNOTS ( 'NONE', 3,
 ( #13690, #9795, #21009, #10052 ),
 .UNSPECIFIED., .F., .F.,
 ( 4, 4 ),
 ( 0.000000000000000000, 0.002452478801916361129 ),
 .UNSPECIFIED. ) ;
#4818 = DIRECTION ( 'NONE',  ( 0.000000000000000000, 2.618450529776313049E-15, 1.000000000000000000 ) ) ;
#4819 = CARTESIAN_POINT ( 'NONE',  ( -14.99999999999998934, -1.734723475976807094E-15, 0.000000000000000000 ) ) ;
#4820 = ORIENTED_EDGE ( 'NONE', *, *, #11656, .T. ) ;
#4821 = EDGE_LOOP ( 'NONE', ( #9709, #11517 ) ) ;
#4822 = DIRECTION ( 'NONE',  ( -1.000000000000000000, -2.775557561562891351E-17, 0.000000000000000000 ) ) ;
#4823 = AXIS2_PLACEMENT_3D ( 'NONE', #20542, #15728, #4616 ) ;
#4824 = EDGE_CURVE ( 'NONE', #3770, #13850, #4854, .T. ) ;
#4825 = DIRECTION ( 'NONE',  ( 0.000000000000000000, 0.000000000000000000, 1.000000000000000000 ) ) ;
#4826 = VECTOR ( 'NONE', #13766, 1000.000000000000000 ) ;
#4827 = EDGE_CURVE ( 'NONE', #12111, #14699, #19000, .T. ) ;
#4828 = CARTESIAN_POINT ( 'NONE',  ( 45.00000000000000000, 272.9999999999999432, 5.249999999999991118 ) ) ;
#4829 = DIRECTION ( 'NONE',  ( 0.000000000000000000, 0.000000000000000000, -1.000000000000000000 ) ) ;
#4830 = CARTESIAN_POINT ( 'NONE',  ( -155.0000000000000284, -494.4690652294806341, 30.00000000000648015 ) ) ;
#4831 = ORIENTED_EDGE ( 'NONE', *, *, #19298, .F. ) ;
#4832 = FACE_OUTER_BOUND ( 'NONE', #20243, .T. ) ;
#4833 = ADVANCED_FACE ( 'NONE', ( #7910 ), #12228, .F. ) ;
#4834 = VERTEX_POINT ( 'NONE', #7790 ) ;
#4835 = AXIS2_PLACEMENT_3D ( 'NONE', #13084, #11378, #11270 ) ;
#4836 = CARTESIAN_POINT ( 'NONE',  ( 4.000000000000000000, -2.309401076758516691, -0.4999999999999995559 ) ) ;
#4837 = CLOSED_SHELL ( 'NONE', ( #20163, #5626, #8681, #22263, #88, #8337, #10668, #10191, #544, #13232, #22991, #23443, #8416, #18584, #14331 ) ) ;
#4838 = CARTESIAN_POINT ( 'NONE',  ( -24.99999999999999645, 9.326071307568738836E-16, -145.0000059999999849 ) ) ;
#4839 = VERTEX_POINT ( 'NONE', #17450 ) ;
#4840 = CARTESIAN_POINT ( 'NONE',  ( 6.523606932381168733, 4.893847819346807348, -7.213065638943126245 ) ) ;
#4841 = FACE_BOUND ( 'NONE', #5806, .T. ) ;
#4842 = ORIENTED_EDGE ( 'NONE', *, *, #21593, .F. ) ;
#4843 = AXIS2_PLACEMENT_3D ( 'NONE', #21224, #6477, #4679 ) ;
#4844 = LINE ( 'NONE', #7455, #7 ) ;
#4845 = LINE ( 'NONE', #4726, #22143 ) ;
#4846 = CONTEXT_DEPENDENT_SHAPE_REPRESENTATION ( #13895, #1780 ) ;
#4847 = ORIENTED_EDGE ( 'NONE', *, *, #5152, .T. ) ;
#4848 = ADVANCED_FACE ( 'NONE', ( #15175 ), #15296, .F. ) ;
#4849 = VECTOR ( 'NONE', #8099, 1000.000000000000000 ) ;
#4850 = CARTESIAN_POINT ( 'NONE',  ( -64.99999999999997158, -52.79999999999974847, 35.00000000000017764 ) ) ;
#4851 = ADVANCED_FACE ( 'NONE', ( #15413 ), #22977, .T. ) ;
#4852 = FACE_BOUND ( 'NONE', #10861, .T. ) ;
#4853 = CARTESIAN_POINT ( 'NONE',  ( -0.6511518506208974211, 8.763486134561267349, -7.907570769506047981 ) ) ;
#4854 = CIRCLE ( 'NONE', #5630, 20.00000000000000000 ) ;
#4855 = DIRECTION ( 'NONE',  ( 0.000000000000000000, -0.8660254037844390407, -0.4999999999999994449 ) ) ;
#4856 = CARTESIAN_POINT ( 'NONE',  ( 52.00000000000000711, -62.00000000000001421, 5.199999999999997513 ) ) ;
#4857 = ORIENTED_EDGE ( 'NONE', *, *, #13940, .F. ) ;
#4858 = CARTESIAN_POINT ( 'NONE',  ( 45.00000000000000000, 250.0000000000000000, -5.249999999999956479 ) ) ;
#4859 =( LENGTH_UNIT ( ) NAMED_UNIT ( * ) SI_UNIT ( .MILLI., .METRE. ) );
#4860 = EDGE_CURVE ( 'NONE', #9995, #1031, #11849, .T. ) ;
#4861 = PRODUCT_DEFINITION_SHAPE ( 'NONE', 'NONE',  #23860 ) ;
#4863 = VERTEX_POINT ( 'NONE', #13743 ) ;
#4862 = ORIENTED_EDGE ( 'NONE', *, *, #20361, .F. ) ;
#4864 = CARTESIAN_POINT ( 'NONE',  ( -44.99999999999998579, -47.79999999999937899, 340.0000000000001705 ) ) ;
#4865 = DIRECTION ( 'NONE',  ( -0.000000000000000000, 0.000000000000000000, -1.000000000000000000 ) ) ;
#4866 = VECTOR ( 'NONE', #10096, 999.9999999999998863 ) ;
#4867 = CARTESIAN_POINT ( 'NONE',  ( 132.8404720734533555, 79.86494211668886578, -32.49999999999351985 ) ) ;
#4868 = CARTESIAN_POINT ( 'NONE',  ( 93.00000000000000000, -74.99999999999998579, 0.000000000000000000 ) ) ;
#4869 = CARTESIAN_POINT ( 'NONE',  ( 1.500000000000000000, 0.000000000000000000, 0.000000000000000000 ) ) ;
#4870 = CARTESIAN_POINT ( 'NONE',  ( -283.1956429438696432, 271.9582675804705332, -145.6220388411722411 ) ) ;
#4871 = EDGE_CURVE ( 'NONE', #18851, #20488, #12999, .T. ) ;
#4872 = VERTEX_POINT ( 'NONE', #20834 ) ;
#4873 = LINE ( 'NONE', #2918, #21876 ) ;
#4874 = ORIENTED_EDGE ( 'NONE', *, *, #10945, .T. ) ;
#4875 = DIRECTION ( 'NONE',  ( 0.000000000000000000, 0.000000000000000000, 1.000000000000000000 ) ) ;
#4876 = CARTESIAN_POINT ( 'NONE',  ( 100.0000000000000000, -1400.000000000000000, 124.9999999999998295 ) ) ;
#4877 = ORIENTED_EDGE ( 'NONE', *, *, #17263, .T. ) ;
#4878 = CARTESIAN_POINT ( 'NONE',  ( -40.00000000000000000, 100.0000000000000000, 150.2000000000009550 ) ) ;
#4879 = ORIENTED_EDGE ( 'NONE', *, *, #5633, .T. ) ;
#4880 = CARTESIAN_POINT ( 'NONE',  ( -24.99999999999998579, -37.41657386773942306, 155.0000000000001705 ) ) ;
#4881 = CARTESIAN_POINT ( 'NONE',  ( 45.00000000000000000, 272.9999999999999432, 0.000000000000000000 ) ) ;
#4882 = VERTEX_POINT ( 'NONE', #4289 ) ;
#4883 = LINE ( 'NONE', #18045, #23251 ) ;
#4884 = DIRECTION ( 'NONE',  ( 0.000000000000000000, -0.000000000000000000, 1.000000000000000000 ) ) ;
#4885 = CARTESIAN_POINT ( 'NONE',  ( -7.894787914004607998, 0.7647108141804108694, -7.591390474663421095 ) ) ;
#4886 = CARTESIAN_POINT ( 'NONE',  ( 30.00000000000000000, 0.000000000000000000, 2.054999999999993054 ) ) ;
#4887 = CARTESIAN_POINT ( 'NONE',  ( -129.2206655591611764, -1072.408698320350140, -29.99999999999356604 ) ) ;
#4888 = CYLINDRICAL_SURFACE ( 'NONE', #10412, 2.649999999999971934 ) ;
#4889 = EDGE_CURVE ( 'NONE', #14699, #6854, #19245, .T. ) ;
#4890 = DIRECTION ( 'NONE',  ( -0.000000000000000000, 1.295896757998781966E-15, 1.000000000000000000 ) ) ;
#4891 = EDGE_CURVE ( 'NONE', #5697, #8918, #11432, .T. ) ;
#4892 = VERTEX_POINT ( 'NONE', #6450 ) ;
#4893 = EDGE_CURVE ( 'NONE', #22939, #13850, #6224, .T. ) ;
#4894 = DIRECTION ( 'NONE',  ( -1.000000000000000000, -2.775557561562891351E-17, -0.000000000000000000 ) ) ;
#4895 = CARTESIAN_POINT ( 'NONE',  ( -4.000000000000000000, 1.677772373332757194, -3.535253723897187506 ) ) ;
#4896 = CIRCLE ( 'NONE', #2183, 5.249999999999973355 ) ;
#4897 = ORIENTED_EDGE ( 'NONE', *, *, #15337, .F. ) ;
#4898 = APPLICATION_CONTEXT ( 'automotive_design' ) ;
#4899 = ORIENTED_EDGE ( 'NONE', *, *, #22306, .F. ) ;
#4900 = DIRECTION ( 'NONE',  ( -1.000000000000000000, -0.000000000000000000, -0.000000000000000000 ) ) ;
#4901 = DIRECTION ( 'NONE',  ( 0.000000000000000000, 0.000000000000000000, 1.000000000000000000 ) ) ;
#4902 = EDGE_CURVE ( 'NONE', #13580, #4142, #13759, .T. ) ;
#4903 = VECTOR ( 'NONE', #2398, 1000.000000000000000 ) ;
#4904 = EDGE_CURVE ( 'NONE', #11935, #12660, #18042, .T. ) ;
#4905 = CARTESIAN_POINT ( 'NONE',  ( -123.1824219776882785, 83.04955713735502343, 30.00000000000641975 ) ) ;
#4906 = CARTESIAN_POINT ( 'NONE',  ( 4.211140560182196957, -2.431303136016555122, -3.745885042887436622 ) ) ;
#4907 = LINE ( 'NONE', #8911, #21178 ) ;
#4908 = EDGE_LOOP ( 'NONE', ( #8011, #817, #5105, #4519 ) ) ;
#4909 = CARTESIAN_POINT ( 'NONE',  ( 1.500000000000000000, 0.000000000000000000, 200.2421591959677016 ) ) ;
#4910 = ORIENTED_EDGE ( 'NONE', *, *, #23370, .F. ) ;
#4911 = CARTESIAN_POINT ( 'NONE',  ( 0.000000000000000000, 2.357898499370434386, -3.469446951953614189E-15 ) ) ;
#4912 = FACE_BOUND ( 'NONE', #15438, .T. ) ;
#4913 = FILL_AREA_STYLE_COLOUR ( '', #5949 ) ;
#4914 = ORIENTED_EDGE ( 'NONE', *, *, #10968, .F. ) ;
#4915 = AXIS2_PLACEMENT_3D ( 'NONE', #17135, #592, #7956 ) ;
#4916 = LINE ( 'NONE', #1037, #16969 ) ;
#4917 = CARTESIAN_POINT ( 'NONE',  ( -175.1609685624536326, -1088.719770019218913, 30.00000000000675726 ) ) ;
#4918 = DIRECTION ( 'NONE',  ( 0.000000000000000000, 0.000000000000000000, 1.000000000000000000 ) ) ;
#4919 = DIRECTION ( 'NONE',  ( 1.000000000000000000, -0.000000000000000000, 6.982962677686266711E-15 ) ) ;
#4921 = AXIS2_PLACEMENT_3D ( 'NONE', #16053, #7204, #6860 ) ;
#4920 = CARTESIAN_POINT ( 'NONE',  ( -3.000000000000002665, 0.000000000000000000, -24.69999999999999929 ) ) ;
#4922 = CARTESIAN_POINT ( 'NONE',  ( 281.4928932188133786, -132.2000000000000455, 177.2000000000014097 ) ) ;
#4923 = DIRECTION ( 'NONE',  ( -0.000000000000000000, 1.000000000000000000, 0.000000000000000000 ) ) ;
#4924 = ORIENTED_EDGE ( 'NONE', *, *, #8154, .F. ) ;
#4925 = ORIENTED_EDGE ( 'NONE', *, *, #5488, .F. ) ;
#4926 = CARTESIAN_POINT ( 'NONE',  ( -281.4928932188134354, 267.8000000000000114, -147.1999999999999318 ) ) ;
#4927 = DIRECTION ( 'NONE',  ( -3.700743415417187942E-15, 1.000000000000000000, 0.000000000000000000 ) ) ;
#4928 = ORIENTED_EDGE ( 'NONE', *, *, #3453, .F. ) ;
#4929 = CARTESIAN_POINT ( 'NONE',  ( -20.00000000000000000, 2.449293598294706513E-15, -150.0000000000000000 ) ) ;
#4930 = DIRECTION ( 'NONE',  ( -0.000000000000000000, 0.000000000000000000, 1.000000000000000000 ) ) ;
#4931 = ADVANCED_FACE ( 'NONE', ( #6694 ), #19724, .T. ) ;
#4932 = EDGE_CURVE ( 'NONE', #22646, #5795, #9894, .T. ) ;
#4933 = AXIS2_PLACEMENT_3D ( 'NONE', #14102, #10595, #3650 ) ;
#4934 = VERTEX_POINT ( 'NONE', #6933 ) ;
#4935 = DIRECTION ( 'NONE',  ( -1.000000000000000000, -0.000000000000000000, -0.000000000000000000 ) ) ;
#4936 = LINE ( 'NONE', #1658, #14563 ) ;
#4937 = VERTEX_POINT ( 'NONE', #12288 ) ;
#4938 = VECTOR ( 'NONE', #513, 1000.000000000000000 ) ;
#4939 = DIRECTION ( 'NONE',  ( -0.000000000000000000, -1.000000000000000000, -0.000000000000000000 ) ) ;
#4940 = VECTOR ( 'NONE', #10337, 1000.000000000000000 ) ;
#4941 = AXIS2_PLACEMENT_3D ( 'NONE', #19828, #3623, #12759 ) ;
#4942 = ORIENTED_EDGE ( 'NONE', *, *, #18044, .F. ) ;
#4943 = DIRECTION ( 'NONE',  ( -0.8090169943749507819, 0.5877852522924686962, 0.000000000000000000 ) ) ;
#4944 =( REPRESENTATION_RELATIONSHIP ('NONE','NONE', #10127, #5587 ) REPRESENTATION_RELATIONSHIP_WITH_TRANSFORMATION ( #18724 )SHAPE_REPRESENTATION_RELATIONSHIP( ) );
#4945 = CARTESIAN_POINT ( 'NONE',  ( 0.000000000000000000, 0.000000000000000000, 0.000000000000000000 ) ) ;
#4946 = ORIENTED_EDGE ( 'NONE', *, *, #15372, .F. ) ;
#4947 = ORIENTED_EDGE ( 'NONE', *, *, #21843, .F. ) ;
#4948 = DIRECTION ( 'NONE',  ( -5.551115123125785858E-15, 5.551115123125785858E-15, -1.000000000000000000 ) ) ;
#4949 = DIRECTION ( 'NONE',  ( 1.000000000000000000, -3.495664435217746987E-15, 0.000000000000000000 ) ) ;
#4950 = CARTESIAN_POINT ( 'NONE',  ( -281.4928932188134354, 267.8000000000000114, -150.1999999999999318 ) ) ;
#4951 = CARTESIAN_POINT ( 'NONE',  ( 126.7787238282394640, 77.44864885511604768, 32.50000000000641620 ) ) ;
#4952 = DIRECTION ( 'NONE',  ( 0.000000000000000000, 0.000000000000000000, 1.000000000000000000 ) ) ;
#4953 = ORIENTED_EDGE ( 'NONE', *, *, #15655, .F. ) ;
#4954 = AXIS2_PLACEMENT_3D ( 'NONE', #5211, #16326, #10916 ) ;
#4955 = CARTESIAN_POINT ( 'NONE',  ( -288.2000000000011255, -29.99999999999898037, -105.0000000000000000 ) ) ;
#4956 = AXIS2_PLACEMENT_3D ( 'NONE', #15563, #22889, #6357 ) ;
#4957 = PRESENTATION_STYLE_ASSIGNMENT (( #848 ) ) ;
#4958 = TOROIDAL_SURFACE ( 'NONE', #5723, 20.30000000000000071, 0.3000000000000059841 ) ;
#4959 = AXIS2_PLACEMENT_3D ( 'NONE', #15194, #2121, #22885 ) ;
#4960 = EDGE_LOOP ( 'NONE', ( #11267, #9945, #18260, #19474 ) ) ;
#4961 = VERTEX_POINT ( 'NONE', #8753 ) ;
#4962 = CARTESIAN_POINT ( 'NONE',  ( -69.99999999999997158, -87.33333333333338544, 3.000000000000001332 ) ) ;
#4963 = ORIENTED_EDGE ( 'NONE', *, *, #7945, .T. ) ;
#4964 = CARTESIAN_POINT ( 'NONE',  ( -146.0000000000000568, -204.4690652294807478, 32.05500000000641592 ) ) ;
#4965 = ORIENTED_EDGE ( 'NONE', *, *, #12548, .T. ) ;
#4966 = PRODUCT_DEFINITION_SHAPE ( 'NONE', 'NONE',  #23810 ) ;
#4967 = CIRCLE ( 'NONE', #3787, 5.249999999999949374 ) ;
#4969 = CIRCLE ( 'NONE', #3791, 2.500000000000000888 ) ;
#4968 = COLOUR_RGB ( '',1.000000000000000000, 0.9490196078431372140, 0.9098039215686274384 ) ;
#4970 = CARTESIAN_POINT ( 'NONE',  ( -59.99999999999996447, -59.80000000000005400, 2.208631632854006084E-13 ) ) ;
#4971 = CIRCLE ( 'NONE', #17321, 7.500000000000002665 ) ;
#4972 = AXIS2_PLACEMENT_3D ( 'NONE', #19995, #6732, #9025 ) ;
#4973 = ORIENTED_EDGE ( 'NONE', *, *, #10568, .T. ) ;
#4974 = DIRECTION ( 'NONE',  ( 1.000000000000000000, 0.000000000000000000, 0.000000000000000000 ) ) ;
#4975 = FILL_AREA_STYLE_COLOUR ( '', #3200 ) ;
#4976 = CONICAL_SURFACE ( 'NONE', #16179, 2.055000000000000160, 0.7853981633974633780 ) ;
#4977 = DIRECTION ( 'NONE',  ( 0.000000000000000000, 0.000000000000000000, 1.000000000000000000 ) ) ;
#4978 = CYLINDRICAL_SURFACE ( 'NONE', #6537, 4.250000000000000000 ) ;
#4979 = CARTESIAN_POINT ( 'NONE',  ( -35.00000000000000711, 4.286263797015737285E-15, -177.2000000000013529 ) ) ;
#4980 = EDGE_LOOP ( 'NONE', ( #18040, #3405, #18711, #1050 ) ) ;
#4981 = DIRECTION ( 'NONE',  ( 1.000000000000000000, 0.000000000000000000, 0.000000000000000000 ) ) ;
#4983 = ORIENTED_EDGE ( 'NONE', *, *, #22838, .F. ) ;
#4982 = EDGE_LOOP ( 'NONE', ( #11522, #8071, #3340, #14686 ) ) ;
#4984 = VECTOR ( 'NONE', #17345, 1000.000000000000114 ) ;
#4985 = DIRECTION ( 'NONE',  ( -8.326672684688674053E-17, 0.000000000000000000, 1.000000000000000000 ) ) ;
#4986 = AXIS2_PLACEMENT_3D ( 'NONE', #13964, #4981, #12044 ) ;
#4987 = FACE_OUTER_BOUND ( 'NONE', #19860, .T. ) ;
#4988 = DIRECTION ( 'NONE',  ( 0.000000000000000000, 0.000000000000000000, 1.000000000000000000 ) ) ;
#4989 = CIRCLE ( 'NONE', #13135, 2.649999999999999467 ) ;
#4990 = CIRCLE ( 'NONE', #8090, 4.250000000000000000 ) ;
#4991 = AXIS2_PLACEMENT_3D ( 'NONE', #4641, #6681, #21296 ) ;
#4992 = CONICAL_SURFACE ( 'NONE', #17707, 2.041999999999999815, 1.047197551196591858 ) ;
#4993 = VECTOR ( 'NONE', #9692, 1000.000000000000000 ) ;
#4994 = CARTESIAN_POINT ( 'NONE',  ( 45.00000000000000000, 250.0000000000000000, 5.249999999999956479 ) ) ;
#4995 = ADVANCED_FACE ( 'NONE', ( #10470 ), #16057, .T. ) ;
#4996 = LINE ( 'NONE', #6319, #12632 ) ;
#4997 = ORIENTED_EDGE ( 'NONE', *, *, #13396, .T. ) ;
#4998 = EDGE_CURVE ( 'NONE', #5086, #10931, #9102, .T. ) ;
#4999 = EDGE_CURVE ( 'NONE', #23312, #8521, #19360, .T. ) ;
#5000 = DIRECTION ( 'NONE',  ( 0.000000000000000000, 0.000000000000000000, 1.000000000000000000 ) ) ;
#5001 = ORIENTED_EDGE ( 'NONE', *, *, #13771, .F. ) ;
#5002 = FACE_OUTER_BOUND ( 'NONE', #7347, .T. ) ;
#5003 = LINE ( 'NONE', #6443, #21197 ) ;
#5004 = EDGE_CURVE ( 'NONE', #1268, #22094, #17809, .T. ) ;
#5005 = ITEM_DEFINED_TRANSFORMATION ( 'NONE', 'NONE', #7327,  #11210 ) ;
#5006 = VERTEX_POINT ( 'NONE', #10701 ) ;
#5007 = CARTESIAN_POINT ( 'NONE',  ( -2.756197834950067094, -3.027510591568735254, -3.223146290109809797 ) ) ;
#5008 = VERTEX_POINT ( 'NONE', #16001 ) ;
#5009 = CARTESIAN_POINT ( 'NONE',  ( -128.9672686250721938, 85.97940096925786690, -28.33934113061009441 ) ) ;
#5010 = DIRECTION ( 'NONE',  ( 0.000000000000000000, 0.000000000000000000, 1.000000000000000000 ) ) ;
#5011 = ADVANCED_BREP_SHAPE_REPRESENTATION ( '', ( #4413, #11210 ), #6181 ) ;
#5012 = VECTOR ( 'NONE', #14087, 1000.000000000000000 ) ;
#5013 = ORIENTED_EDGE ( 'NONE', *, *, #13507, .F. ) ;
#5014 = FILL_AREA_STYLE ('',( #18164 ) ) ;
#5015 =( GEOMETRIC_REPRESENTATION_CONTEXT ( 3 ) GLOBAL_UNCERTAINTY_ASSIGNED_CONTEXT ( ( #22660 ) ) GLOBAL_UNIT_ASSIGNED_CONTEXT ( ( #3030, #21289, #23324 ) ) REPRESENTATION_CONTEXT ( 'NONE', 'WORKASPACE' ) );
#5016 = LINE ( 'NONE', #21069, #19220 ) ;
#5017 = VECTOR ( 'NONE', #17639, 1000.000000000000000 ) ;
#5018 = VECTOR ( 'NONE', #15077, 1000.000000000000000 ) ;
#5019 = CARTESIAN_POINT ( 'NONE',  ( 1.567478505476134606E-15, 4.618802153517012066, -5.000000000000000000 ) ) ;
#5020 = DIRECTION ( 'NONE',  ( 0.000000000000000000, 0.000000000000000000, -1.000000000000000000 ) ) ;
#5021 = CARTESIAN_POINT ( 'NONE',  ( 32.35000000000000142, 90.00000000000000000, 3.000000000000001332 ) ) ;
#5022 = CARTESIAN_POINT ( 'NONE',  ( -285.2000000000008981, 30.00000000000101963, -102.3500000000000369 ) ) ;
#5023 = DIRECTION ( 'NONE',  ( -0.9510565162951557516, 0.3090169943749406234, 0.000000000000000000 ) ) ;
#5024 = ORIENTED_EDGE ( 'NONE', *, *, #18551, .T. ) ;
#5025 =( NAMED_UNIT ( * ) PLANE_ANGLE_UNIT ( ) SI_UNIT ( $, .RADIAN. ) );
#5026 = DIRECTION ( 'NONE',  ( -6.982962677686266711E-15, 0.000000000000000000, 1.000000000000000000 ) ) ;
#5027 = DIRECTION ( 'NONE',  ( -0.000000000000000000, -0.000000000000000000, 1.000000000000000000 ) ) ;
#5028 = ORIENTED_EDGE ( 'NONE', *, *, #4871, .F. ) ;
#5029 = ORIENTED_EDGE ( 'NONE', *, *, #11277, .T. ) ;
#5030 = DIRECTION ( 'NONE',  ( 0.000000000000000000, 1.000000000000000000, 0.000000000000000000 ) ) ;
#5031 = DIRECTION ( 'NONE',  ( -3.469446951953614682E-16, 1.000000000000000000, -3.483493295888648978E-15 ) ) ;
#5032 = CARTESIAN_POINT ( 'NONE',  ( -5.007715329123872641E-16, -8.660254037844399733, -10.00000000000000000 ) ) ;
#5033 = CIRCLE ( 'NONE', #10063, 2.700000000000000622 ) ;
#5034 = CIRCLE ( 'NONE', #16228, 7.500000000000002665 ) ;
#5035 = CARTESIAN_POINT ( 'NONE',  ( 0.000000000000000000, 1.178949249685212974, -2.042000000000001148 ) ) ;
#5036 = CIRCLE ( 'NONE', #7736, 5.249999999999949374 ) ;
#5037 = ADVANCED_FACE ( 'NONE', ( #1135 ), #8520, .T. ) ;
#5038 = FACE_OUTER_BOUND ( 'NONE', #6189, .T. ) ;
#5039 = CARTESIAN_POINT ( 'NONE',  ( -146.0000000000005116, -204.4690652294800657, -29.99999999999356604 ) ) ;
#5040 = ADVANCED_FACE ( 'NONE', ( #5121 ), #6389, .T. ) ;
#5041 = EDGE_LOOP ( 'NONE', ( #2123, #3141, #18929, #11376 ) ) ;
#5042 = CYLINDRICAL_SURFACE ( 'NONE', #21603, 9.999999999999998224 ) ;
#5043 = ADVANCED_FACE ( 'NONE', ( #23591 ), #16117, .F. ) ;
#5044 = ORIENTED_EDGE ( 'NONE', *, *, #21440, .T. ) ;
#5045 = CARTESIAN_POINT ( 'NONE',  ( -7.500000000000000000, 4.330127018922191873, -7.422398894150032511 ) ) ;
#5046 = DIRECTION ( 'NONE',  ( -1.000000000000000000, -0.000000000000000000, -0.000000000000000000 ) ) ;
#5047 = LINE ( 'NONE', #3556, #4396 ) ;
#5048 = EDGE_LOOP ( 'NONE', ( #4928, #7759, #12379, #19509 ) ) ;
#5049 = DIRECTION ( 'NONE',  ( 0.000000000000000000, -0.4999999999999993894, 0.8660254037844389297 ) ) ;
#5050 = EDGE_CURVE ( 'NONE', #17172, #5473, #20265, .T. ) ;
#5051 = CARTESIAN_POINT ( 'NONE',  ( 285.2000000000013529, -127.0000000000000568, -146.4928932188134070 ) ) ;
#5052 = CARTESIAN_POINT ( 'NONE',  ( 1.500000000000000000, 11.99999999999999822, 150.0000000000000284 ) ) ;
#5053 = CARTESIAN_POINT ( 'NONE',  ( -35.00000000000000711, 4.286263797015349166E-15, -147.2000000000008981 ) ) ;
#5054 = ADVANCED_FACE ( 'NONE', ( #11063 ), #14794, .F. ) ;
#5055 = FACE_OUTER_BOUND ( 'NONE', #1079, .T. ) ;
#5056 = CARTESIAN_POINT ( 'NONE',  ( 171.6502151485116485, 95.33502053007514121, -29.99999999999322498 ) ) ;
#5057 = CARTESIAN_POINT ( 'NONE',  ( 0.000000000000000000, 0.000000000000000000, 0.000000000000000000 ) ) ;
#5058 = VERTEX_POINT ( 'NONE', #21773 ) ;
#5059 = ORIENTED_EDGE ( 'NONE', *, *, #9120, .F. ) ;
#5060 = DIRECTION ( 'NONE',  ( 0.000000000000000000, 0.000000000000000000, -1.000000000000000000 ) ) ;
#5061 = CARTESIAN_POINT ( 'NONE',  ( 281.3673129565597151, 268.0906609804447385, 147.1854425596106921 ) ) ;
#5062 = ORIENTED_EDGE ( 'NONE', *, *, #17138, .F. ) ;
#5063 = FACE_OUTER_BOUND ( 'NONE', #3303, .T. ) ;
#5064 = DIRECTION ( 'NONE',  ( 0.000000000000000000, 1.177509268541832635E-16, -1.000000000000000000 ) ) ;
#5065 = ORIENTED_EDGE ( 'NONE', *, *, #10407, .T. ) ;
#5066 = CARTESIAN_POINT ( 'NONE',  ( 281.4928932188133217, 267.7999999999999545, 150.2299999999999898 ) ) ;
#5067 = CARTESIAN_POINT ( 'NONE',  ( -45.00000000000000000, 269.9999999999999432, 0.000000000000000000 ) ) ;
#5068 = VERTEX_POINT ( 'NONE', #12067 ) ;
#5069 = DIRECTION ( 'NONE',  ( 1.000000000000000000, 0.000000000000000000, 0.000000000000000000 ) ) ;
#5070 = ORIENTED_EDGE ( 'NONE', *, *, #1975, .T. ) ;
#5071 = DIRECTION ( 'NONE',  ( -0.000000000000000000, -0.000000000000000000, 1.000000000000000000 ) ) ;
#5072 = EDGE_LOOP ( 'NONE', ( #21356, #3944, #6775, #20068 ) ) ;
#5073 = VERTEX_POINT ( 'NONE', #2820 ) ;
#5074 = CARTESIAN_POINT ( 'NONE',  ( 133.1760469597745669, 79.30426557766901396, -27.57920702976964122 ) ) ;
#5075 = PRODUCT_DEFINITION_SHAPE ( 'NONE', 'NONE',  #23823 ) ;
#5076 = APPLICATION_PROTOCOL_DEFINITION ( 'draft international standard', 'automotive_design', 1998, #15572 ) ;
#5077 = CARTESIAN_POINT ( 'NONE',  ( -281.3681929792554115, 268.4822561791010003, -150.1663407402828909 ) ) ;
#5078 = EDGE_CURVE ( 'NONE', #13410, #12660, #8384, .T. ) ;
#5079 = ADVANCED_FACE ( 'NONE', ( #6585 ), #2902, .F. ) ;
#5080 = ADVANCED_FACE ( 'NONE', ( #2928 ), #12174, .F. ) ;
#5081 = DIRECTION ( 'NONE',  ( 1.000000000000000000, 0.000000000000000000, 0.000000000000000000 ) ) ;
#5082 = CYLINDRICAL_SURFACE ( 'NONE', #14031, 2.500000000000002220 ) ;
#5083 = ORIENTED_EDGE ( 'NONE', *, *, #14322, .F. ) ;
#5084 = DIRECTION ( 'NONE',  ( 0.000000000000000000, -1.000000000000000000, -1.177509268541832635E-16 ) ) ;
#5085 = ORIENTED_EDGE ( 'NONE', *, *, #6210, .T. ) ;
#5086 = VERTEX_POINT ( 'NONE', #20086 ) ;
#5087 = LINE ( 'NONE', #21846, #20686 ) ;
#5088 = EDGE_LOOP ( 'NONE', ( #1020, #15111, #16638, #3063, #3619, #20428, #19414, #20248 ) ) ;
#5089 = DIRECTION ( 'NONE',  ( 0.000000000000000000, 0.000000000000000000, -1.000000000000000000 ) ) ;
#5090 = B_SPLINE_CURVE_WITH_KNOTS ( 'NONE', 3,
 ( #823, #6621, #19289, #2853, #14250, #2753, #12462, #17844, #2971, #23390, #10255, #8558, #8429, #15689, #22901, #10509, #17594, #1049, #19762, #21343 ),
 .UNSPECIFIED., .F., .F.,
 ( 4, 2, 2, 2, 2, 2, 2, 2, 2, 4 ),
 ( 0.000000000000000000, 0.001035985217005883649, 0.002071970434011767299, 0.003107955651017651165, 0.003625948259520570330, 0.004143940868023489495, 0.005179926085029110984, 0.006215911302034731606, 0.007251896519040352228, 0.008287881736045972850 ),
 .UNSPECIFIED. ) ;
#5091 = ORIENTED_EDGE ( 'NONE', *, *, #1894, .T. ) ;
#5092 = FACE_OUTER_BOUND ( 'NONE', #8733, .T. ) ;
#5093 = ORIENTED_EDGE ( 'NONE', *, *, #4688, .F. ) ;
#5094 = CARTESIAN_POINT ( 'NONE',  ( -1.655952806101422814, 3.662737355149034979, -7.623296525288699970E-18 ) ) ;
#5095 = EDGE_CURVE ( 'NONE', #10369, #6737, #3639, .T. ) ;
#5096 = DIRECTION ( 'NONE',  ( 5.050510105632271307E-15, -4.822252111914687128E-15, 1.000000000000000000 ) ) ;
#5097 = DIRECTION ( 'NONE',  ( 0.000000000000000000, 0.000000000000000000, 1.000000000000000000 ) ) ;
#5098 = EDGE_CURVE ( 'NONE', #23584, #18606, #1752, .T. ) ;
#5099 = CARTESIAN_POINT ( 'NONE',  ( 99.99999999999987210, -129.2000000000000455, 152.4000000000014268 ) ) ;
#5100 = ORIENTED_EDGE ( 'NONE', *, *, #23412, .F. ) ;
#5101 = PLANE ( 'NONE',  #678 ) ;
#5102 = FILL_AREA_STYLE ('',( #10446 ) ) ;
#5103 = AXIS2_PLACEMENT_3D ( 'NONE', #3974, #11388, #2164 ) ;
#5105 = ORIENTED_EDGE ( 'NONE', *, *, #15119, .T. ) ;
#5104 = EDGE_LOOP ( 'NONE', ( #4220, #18245, #19362, #17110 ) ) ;
#5106 = DIRECTION ( 'NONE',  ( 1.000000000000000000, 0.000000000000000000, 6.123233995736766036E-17 ) ) ;
#5107 = LINE ( 'NONE', #3278, #23525 ) ;
#5108 = DIRECTION ( 'NONE',  ( -0.000000000000000000, -0.000000000000000000, -1.000000000000000000 ) ) ;
#5109 = DIRECTION ( 'NONE',  ( 1.000000000000000000, 0.000000000000000000, 0.000000000000000000 ) ) ;
#5110 = DIRECTION ( 'NONE',  ( 1.000000000000000000, -0.000000000000000000, 6.982962677686266711E-15 ) ) ;
#5111 = VERTEX_POINT ( 'NONE', #13000 ) ;
#5112 = DIRECTION ( 'NONE',  ( 0.000000000000000000, 0.000000000000000000, -1.000000000000000000 ) ) ;
#5113 = ORIENTED_EDGE ( 'NONE', *, *, #22098, .T. ) ;
#5114 = CARTESIAN_POINT ( 'NONE',  ( -2.352990130084580066E-16, 8.660254037844390851, -10.00000000000000000 ) ) ;
#5115 = CYLINDRICAL_SURFACE ( 'NONE', #1499, 45.00000000000000711 ) ;
#5116 = EDGE_CURVE ( 'NONE', #3094, #19888, #21883, .T. ) ;
#5117 = ORIENTED_EDGE ( 'NONE', *, *, #11925, .T. ) ;
#5118 = CIRCLE ( 'NONE', #12495, 2.649999999999985700 ) ;
#5119 = ORIENTED_EDGE ( 'NONE', *, *, #8437, .F. ) ;
#5120 = CARTESIAN_POINT ( 'NONE',  ( -127.9021285790837510, 87.55595642181941685, -32.49999999999351985 ) ) ;
#5121 = FACE_OUTER_BOUND ( 'NONE', #5447, .T. ) ;
#5122 = EDGE_LOOP ( 'NONE', ( #14317, #14513, #3462, #9489 ) ) ;
#5123 = CARTESIAN_POINT ( 'NONE',  ( -280.8706349181170481, 270.9682701916305518, 149.1268706878666706 ) ) ;
#5124 = CARTESIAN_POINT ( 'NONE',  ( -7.499999999999999112, 34.18698582794336716, 100.0000000000000000 ) ) ;
#5125 = DIRECTION ( 'NONE',  ( -0.000000000000000000, -0.000000000000000000, 1.000000000000000000 ) ) ;
#5126 = CARTESIAN_POINT ( 'NONE',  ( 100.0000000000000000, -1420.000000000000000, 144.9999999999998295 ) ) ;
#5127 = CARTESIAN_POINT ( 'NONE',  ( -4.198928548860774157, 0.8158838809860065044, -3.526471437616918170 ) ) ;
#5128 = CARTESIAN_POINT ( 'NONE',  ( 137.9031948627977044, -44.80746418436605438, 90.00000000000000000 ) ) ;
#5129 = EDGE_CURVE ( 'NONE', #3613, #23122, #19882, .T. ) ;
#5130 = CARTESIAN_POINT ( 'NONE',  ( -146.0000000000000853, -204.4690652294807478, 30.00000000000641620 ) ) ;
#5131 = ORIENTED_EDGE ( 'NONE', *, *, #1479, .T. ) ;
#5132 = CARTESIAN_POINT ( 'NONE',  ( -7.500000000000000888, -3.608439182435167591, -7.298562697733108173 ) ) ;
#5133 = CARTESIAN_POINT ( 'NONE',  ( -1.243802165048909503, 3.900692638707381921, -3.223146290109805800 ) ) ;
#5134 = EDGE_CURVE ( 'NONE', #11791, #2882, #7512, .T. ) ;
#5135 = VECTOR ( 'NONE', #17355, 1000.000000000000000 ) ;
#5136 = EDGE_LOOP ( 'NONE', ( #19706, #11947, #11406, #8098 ) ) ;
#5137 = DIRECTION ( 'NONE',  ( 1.000000000000000000, -3.495664435217746987E-15, -0.000000000000000000 ) ) ;
#5138 = DIRECTION ( 'NONE',  ( -1.000000000000000000, -0.000000000000000000, -0.000000000000000000 ) ) ;
#5139 = CARTESIAN_POINT ( 'NONE',  ( -282.1697000000000912, 267.7999999999999545, 146.4928932188134354 ) ) ;
#5140 = CARTESIAN_POINT ( 'NONE',  ( -100.0000000000000000, 35.00000000000009948, -113.4834095219707848 ) ) ;
#5141 = FACE_OUTER_BOUND ( 'NONE', #13713, .T. ) ;
#5142 = ORIENTED_EDGE ( 'NONE', *, *, #3127, .F. ) ;
#5144 = VECTOR ( 'NONE', #15534, 1000.000000000000000 ) ;
#5143 = FACE_OUTER_BOUND ( 'NONE', #12319, .T. ) ;
#5145 = ORIENTED_EDGE ( 'NONE', *, *, #18703, .T. ) ;
#5146 = LINE ( 'NONE', #23615, #12616 ) ;
#5147 = LINE ( 'NONE', #19985, #7654 ) ;
#5148 = AXIS2_PLACEMENT_3D ( 'NONE', #7883, #6305, #19333 ) ;
#5149 = EDGE_LOOP ( 'NONE', ( #12095, #20069, #780, #1125 ) ) ;
#5150 = AXIS2_PLACEMENT_3D ( 'NONE', #19484, #21427, #3074 ) ;
#5151 = LINE ( 'NONE', #10249, #9559 ) ;
#5152 = EDGE_CURVE ( 'NONE', #422, #15868, #3893, .T. ) ;
#5153 = FACE_OUTER_BOUND ( 'NONE', #14025, .T. ) ;
#5154 = LINE ( 'NONE', #3458, #12910 ) ;
#5155 = EDGE_CURVE ( 'NONE', #22350, #18427, #1962, .T. ) ;
#5156 = FACE_OUTER_BOUND ( 'NONE', #18447, .T. ) ;
#5157 = PLANE ( 'NONE',  #20763 ) ;
#5158 = DIRECTION ( 'NONE',  ( -1.000000000000000000, -0.000000000000000000, -0.000000000000000000 ) ) ;
#5159 = EDGE_LOOP ( 'NONE', ( #22553, #4290, #12848, #10050 ) ) ;
#5160 = VERTEX_POINT ( 'NONE', #15024 ) ;
#5161 = CYLINDRICAL_SURFACE ( 'NONE', #3364, 2.649999999999971934 ) ;
#5162 = DIRECTION ( 'NONE',  ( 1.000000000000000000, 0.000000000000000000, 0.000000000000000000 ) ) ;
#5163 = ADVANCED_FACE ( 'NONE', ( #20435 ), #19957, .F. ) ;
#5164 = ORIENTED_EDGE ( 'NONE', *, *, #3086, .F. ) ;
#5165 = AXIS2_PLACEMENT_3D ( 'NONE', #6280, #6639, #19061 ) ;
#5166 = EDGE_CURVE ( 'NONE', #1715, #17062, #9285, .T. ) ;
#5167 = PRODUCT_DEFINITION_SHAPE ( 'NONE', 'NONE',  #23817 ) ;
#5168 = DIRECTION ( 'NONE',  ( 0.000000000000000000, 0.000000000000000000, 1.000000000000000000 ) ) ;
#5170 = CIRCLE ( 'NONE', #11755, 2.649999999999999467 ) ;
#5169 = PLANE ( 'NONE',  #3369 ) ;
#5171 = ORIENTED_EDGE ( 'NONE', *, *, #18009, .F. ) ;
#5172 = CARTESIAN_POINT ( 'NONE',  ( -40.00000000000000000, 100.0000000000000000, -145.0000000000000284 ) ) ;
#5173 = EDGE_CURVE ( 'NONE', #11003, #949, #53, .T. ) ;
#5174 = CARTESIAN_POINT ( 'NONE',  ( -5.878907051488763358, 8.175524754488199264, 200.0000119999999981 ) ) ;
#5175 = ORIENTED_EDGE ( 'NONE', *, *, #23379, .F. ) ;
#5176 = PLANE ( 'NONE',  #16406 ) ;
#5177 = ORIENTED_EDGE ( 'NONE', *, *, #20562, .F. ) ;
#5178 = CARTESIAN_POINT ( 'NONE',  ( 235.0000000000000284, -499.9999999999998863, 60.00000000000002132 ) ) ;
#5179 = CARTESIAN_POINT ( 'NONE',  ( -155.0000000000000284, -204.4690652294799520, -29.99999999999350564 ) ) ;
#5180 = DIRECTION ( 'NONE',  ( 3.469446951953614682E-16, -1.000000000000000000, 3.483493295888648978E-15 ) ) ;
#5181 = ORIENTED_EDGE ( 'NONE', *, *, #22626, .F. ) ;
#5182 = EDGE_LOOP ( 'NONE', ( #12131, #9938, #6429, #12883 ) ) ;
#5183 = CARTESIAN_POINT ( 'NONE',  ( -123.1824219776881648, 83.04955713735580503, -29.99999999999356248 ) ) ;
#5184 = AXIS2_PLACEMENT_3D ( 'NONE', #4791, #691, #12204 ) ;
#5185 = DIRECTION ( 'NONE',  ( -1.000000000000000000, 0.000000000000000000, 6.123233995736766036E-17 ) ) ;
#5186 = CARTESIAN_POINT ( 'NONE',  ( -126.5033273815582220, 89.56511165728103663, -29.34813586885359626 ) ) ;
#5187 = CIRCLE ( 'NONE', #23681, 21.02499999999999858 ) ;
#5188 = DIRECTION ( 'NONE',  ( 0.000000000000000000, -1.000000000000000000, 0.000000000000000000 ) ) ;
#5189 = VECTOR ( 'NONE', #237, 1000.000000000000000 ) ;
#5190 = DIRECTION ( 'NONE',  ( -0.7232617928448825673, 0.6905739489807055653, 6.982962677686265922E-15 ) ) ;
#5191 = EDGE_LOOP ( 'NONE', ( #22391, #352, #7597, #5517 ) ) ;
#5192 = EDGE_CURVE ( 'NONE', #13453, #2982, #16348, .T. ) ;
#5193 = FACE_OUTER_BOUND ( 'NONE', #90, .T. ) ;
#5194 = ADVANCED_FACE ( 'NONE', ( #7157 ), #11532, .F. ) ;
#5195 = ORIENTED_EDGE ( 'NONE', *, *, #31, .F. ) ;
#5196 = ADVANCED_FACE ( 'NONE', ( #754 ), #13714, .F. ) ;
#5197 = DIRECTION ( 'NONE',  ( -1.000000000000000000, 0.000000000000000000, -0.000000000000000000 ) ) ;
#5198 = DIRECTION ( 'NONE',  ( 0.000000000000000000, 0.000000000000000000, 1.000000000000000000 ) ) ;
#5199 = AXIS2_PLACEMENT_3D ( 'NONE', #3664, #14930, #1855 ) ;
#5200 = ADVANCED_FACE ( 'NONE', ( #862, #17182, #4120 ), #20666, .F. ) ;
#5201 = ORIENTED_EDGE ( 'NONE', *, *, #8482, .T. ) ;
#5203 = ADVANCED_FACE ( 'NONE', ( #17063 ), #9947, .F. ) ;
#5202 = DIRECTION ( 'NONE',  ( 0.000000000000000000, 1.334402673828305746E-15, -1.000000000000000000 ) ) ;
#5204 =( GEOMETRIC_REPRESENTATION_CONTEXT ( 3 ) GLOBAL_UNCERTAINTY_ASSIGNED_CONTEXT ( ( #824 ) ) GLOBAL_UNIT_ASSIGNED_CONTEXT ( ( #13578, #13439, #22330 ) ) REPRESENTATION_CONTEXT ( 'NONE', 'WORKASPACE' ) );
#5205 = VECTOR ( 'NONE', #8406, 1000.000000000000000 ) ;
#5206 = EDGE_LOOP ( 'NONE', ( #6622, #21358, #10468, #15696 ) ) ;
#5207 = DIRECTION ( 'NONE',  ( 0.000000000000000000, 0.000000000000000000, -1.000000000000000000 ) ) ;
#5208 = EDGE_LOOP ( 'NONE', ( #20286, #13243, #23748 ) ) ;
#5209 = CARTESIAN_POINT ( 'NONE',  ( 10.39117206796836257, 0.000000000000000000, -8.499999999999998224 ) ) ;
#5210 = CARTESIAN_POINT ( 'NONE',  ( -280.9954397628185916, 268.9021437883071712, 146.9094021484633856 ) ) ;
#5211 = CARTESIAN_POINT ( 'NONE',  ( -105.0000000000000000, -29.99999999999998579, 3.000000000000001332 ) ) ;
#5212 = CARTESIAN_POINT ( 'NONE',  ( 0.000000000000000000, 0.000000000000000000, -4.484454397937119197 ) ) ;
#5213 = AXIS2_PLACEMENT_3D ( 'NONE', #18430, #9158, #10637 ) ;
#5214 = ADVANCED_FACE ( 'NONE', ( #17423 ), #2187, .F. ) ;
#5215 = DIRECTION ( 'NONE',  ( 0.000000000000000000, 1.000000000000000000, -4.183096374613631247E-18 ) ) ;
#5216 = VERTEX_POINT ( 'NONE', #2321 ) ;
#5217 = CARTESIAN_POINT ( 'NONE',  ( 0.2500000000000002220, 4.898587196589412829E-16, -4.000000000000000000 ) ) ;
#5218 =( NAMED_UNIT ( * ) SI_UNIT ( $, .STERADIAN. ) SOLID_ANGLE_UNIT ( ) );
#5219 = AXIS2_PLACEMENT_3D ( 'NONE', #9427, #4343, #13213 ) ;
#5221 = EDGE_LOOP ( 'NONE', ( #16159, #9471, #6726, #17758 ) ) ;
#5220 = EDGE_LOOP ( 'NONE', ( #16379, #14086, #2626, #6872 ) ) ;
#5222 = DIRECTION ( 'NONE',  ( -1.000000000000000000, 3.495664435217746987E-15, 0.000000000000000000 ) ) ;
#5223 = LINE ( 'NONE', #1355, #14298 ) ;
#5224 = DIRECTION ( 'NONE',  ( 0.000000000000000000, 0.000000000000000000, 1.000000000000000000 ) ) ;
#5225 = ORIENTED_EDGE ( 'NONE', *, *, #15117, .T. ) ;
#5226 = FACE_OUTER_BOUND ( 'NONE', #20922, .T. ) ;
#5227 = EDGE_CURVE ( 'NONE', #18517, #6982, #11665, .T. ) ;
#5228 = CIRCLE ( 'NONE', #18315, 160.0000000000000000 ) ;
#5229 = VERTEX_POINT ( 'NONE', #6194 ) ;
#5230 = EDGE_CURVE ( 'NONE', #20797, #21004, #13779, .T. ) ;
#5231 = FACE_OUTER_BOUND ( 'NONE', #22622, .T. ) ;
#5232 = ADVANCED_FACE ( 'NONE', ( #18970 ), #7881, .F. ) ;
#5233 = ORIENTED_EDGE ( 'NONE', *, *, #18462, .F. ) ;
#5234 = LINE ( 'NONE', #10695, #15031 ) ;
#5235 = LINE ( 'NONE', #12641, #12741 ) ;
#5236 = ITEM_DEFINED_TRANSFORMATION ( 'NONE', 'NONE', #15832,  #11210 ) ;
#5237 = VERTEX_POINT ( 'NONE', #13605 ) ;
#5238 = VECTOR ( 'NONE', #13632, 1000.000000000000000 ) ;
#5239 = EDGE_LOOP ( 'NONE', ( #5299, #10607, #12301, #1609 ) ) ;
#5240 = CARTESIAN_POINT ( 'NONE',  ( -20.63749999999999929, 2.574819895207309803E-15, 21.02499999999999503 ) ) ;
#5241 = ORIENTED_EDGE ( 'NONE', *, *, #2778, .T. ) ;
#5242 = CARTESIAN_POINT ( 'NONE',  ( -7.499999999999999112, 34.18698582794336716, 100.0000000000000000 ) ) ;
#5243 = CARTESIAN_POINT ( 'NONE',  ( -7.499999999999999112, 34.18698582794336716, 100.0000000000000000 ) ) ;
#5244 = DIRECTION ( 'NONE',  ( 0.000000000000000000, 0.000000000000000000, -1.000000000000000000 ) ) ;
#5245 = DIRECTION ( 'NONE',  ( -1.000000000000000000, -0.000000000000000000, -0.000000000000000000 ) ) ;
#5246 = DIRECTION ( 'NONE',  ( -1.000000000000000000, -3.469446951953614682E-16, -0.000000000000000000 ) ) ;
#5247 = VECTOR ( 'NONE', #22265, 1000.000000000000000 ) ;
#5248 = FACE_OUTER_BOUND ( 'NONE', #1372, .T. ) ;
#5249 = VERTEX_POINT ( 'NONE', #4496 ) ;
#5250 =( NAMED_UNIT ( * ) PLANE_ANGLE_UNIT ( ) SI_UNIT ( $, .RADIAN. ) );
#5251 = CARTESIAN_POINT ( 'NONE',  ( -7.500000000000000000, 4.330127018922191873, -7.422398894150032511 ) ) ;
#5252 = FACE_OUTER_BOUND ( 'NONE', #5264, .T. ) ;
#5253 = ORIENTED_EDGE ( 'NONE', *, *, #7872, .T. ) ;
#5254 = DIRECTION ( 'NONE',  ( -1.000000000000000000, 0.000000000000000000, 0.000000000000000000 ) ) ;
#5255 = LINE ( 'NONE', #6957, #23747 ) ;
#5256 = ADVANCED_BREP_SHAPE_REPRESENTATION ( '', ( #19781, #11210 ), #5408 ) ;
#5257 = DIRECTION ( 'NONE',  ( 0.000000000000000000, -1.000000000000000000, 1.287488025362403787E-15 ) ) ;
#5258 = CIRCLE ( 'NONE', #10281, 2.649999999999978595 ) ;
#5259 = FACE_OUTER_BOUND ( 'NONE', #23081, .T. ) ;
#5260 = DIRECTION ( 'NONE',  ( -0.7232617928448825673, 0.6905739489807055653, 6.982962677686266711E-15 ) ) ;
#5261 = AXIS2_PLACEMENT_3D ( 'NONE', #17011, #7818, #5777 ) ;
#5262 = VERTEX_POINT ( 'NONE', #16944 ) ;
#5263 = CARTESIAN_POINT ( 'NONE',  ( 0.000000000000000000, 0.000000000000000000, -90.00000000000000000 ) ) ;
#5264 = EDGE_LOOP ( 'NONE', ( #15057, #3012, #2985, #7404 ) ) ;
#5265 = CARTESIAN_POINT ( 'NONE',  ( 0.000000000000000000, 0.000000000000000000, -4.694516984716113228 ) ) ;
#5266 = CARTESIAN_POINT ( 'NONE',  ( 0.000000000000000000, 0.000000000000000000, 3.000000000000000000 ) ) ;
#5267 = FILL_AREA_STYLE ('',( #8784 ) ) ;
#5268 = EDGE_LOOP ( 'NONE', ( #6337, #19567, #21082, #1051 ) ) ;
#5269 = CARTESIAN_POINT ( 'NONE',  ( -288.2000000000013529, -89.99999999999897682, 24.33333333333333215 ) ) ;
#5270 = CARTESIAN_POINT ( 'NONE',  ( 34.75000000000005684, 100.0000000000000000, -145.0000000000000284 ) ) ;
#5271 = CARTESIAN_POINT ( 'NONE',  ( -3.749999999999998224, -6.495190528383296247, -6.991905250253752868 ) ) ;
#5272 = CARTESIAN_POINT ( 'NONE',  ( 1.970645868709654753E-14, -56.80000000000003268, 2.055021403285669549E-13 ) ) ;
#5273 = DIRECTION ( 'NONE',  ( 0.8191520442889907994, 1.003171929053523514E-16, -0.5735764363510474917 ) ) ;
#5274 = FACE_OUTER_BOUND ( 'NONE', #9419, .T. ) ;
#5275 = PLANE ( 'NONE',  #7839 ) ;
#5276 = ORIENTED_EDGE ( 'NONE', *, *, #9577, .F. ) ;
#5277 = ORIENTED_EDGE ( 'NONE', *, *, #11315, .F. ) ;
#5278 = LINE ( 'NONE', #16389, #8786 ) ;
#5279 = CIRCLE ( 'NONE', #18747, 19.99999999999998934 ) ;
#5280 = LINE ( 'NONE', #18418, #16583 ) ;
#5281 = ORIENTED_EDGE ( 'NONE', *, *, #20668, .T. ) ;
#5282 = DIRECTION ( 'NONE',  ( 0.000000000000000000, 0.000000000000000000, -1.000000000000000000 ) ) ;
#5283 = FACE_OUTER_BOUND ( 'NONE', #4042, .T. ) ;
#5284 = EDGE_LOOP ( 'NONE', ( #10922, #18845, #2299, #18557 ) ) ;
#5285 = CARTESIAN_POINT ( 'NONE',  ( 0.000000000000000000, -1000.000000000000000, -145.0000119999999697 ) ) ;
#5286 = EDGE_CURVE ( 'NONE', #17629, #7103, #2557, .T. ) ;
#5287 = LINE ( 'NONE', #3225, #3722 ) ;
#5288 = EDGE_LOOP ( 'NONE', ( #18687, #1653, #22937, #6586 ) ) ;
#5289 = DIRECTION ( 'NONE',  ( -0.5877852522924643663, -0.8090169943749537795, 0.000000000000000000 ) ) ;
#5290 = ADVANCED_FACE ( 'NONE', ( #11780 ), #19093, .T. ) ;
#5291 = EDGE_CURVE ( 'NONE', #10553, #13555, #8137, .T. ) ;
#5292 = VECTOR ( 'NONE', #19917, 1000.000000000000114 ) ;
#5293 = ORIENTED_EDGE ( 'NONE', *, *, #22472, .T. ) ;
#5294 = CARTESIAN_POINT ( 'NONE',  ( 281.4928932188134354, -132.2000000000000455, -152.4000000000012847 ) ) ;
#5295 = CARTESIAN_POINT ( 'NONE',  ( -136.8705256357205258, -1072.742444906769151, 31.11216498479345205 ) ) ;
#5296 = VECTOR ( 'NONE', #22077, 1000.000000000000000 ) ;
#5297 = EDGE_CURVE ( 'NONE', #9785, #20023, #6407, .T. ) ;
#5298 = DIRECTION ( 'NONE',  ( -1.000000000000000000, 0.000000000000000000, 0.000000000000000000 ) ) ;
#5299 = ORIENTED_EDGE ( 'NONE', *, *, #16396, .T. ) ;
#5300 = VERTEX_POINT ( 'NONE', #6304 ) ;
#5301 = CARTESIAN_POINT ( 'NONE',  ( 0.000000000000000000, 0.000000000000000000, -177.2000000000013529 ) ) ;
#5302 = CARTESIAN_POINT ( 'NONE',  ( -126.6049454172958377, 89.42142849841020791, -28.88783501520649111 ) ) ;
#5303 = DIRECTION ( 'NONE',  ( 1.000000000000000000, 0.000000000000000000, 0.000000000000000000 ) ) ;
#5304 = DIRECTION ( 'NONE',  ( -0.000000000000000000, -0.000000000000000000, -1.000000000000000000 ) ) ;
#5305 = EDGE_LOOP ( 'NONE', ( #17054, #16245 ) ) ;
#5306 = CARTESIAN_POINT ( 'NONE',  ( 8.055391459054622061, -23.72315261474502890, 145.0000119999999697 ) ) ;
#5307 = PRESENTATION_STYLE_ASSIGNMENT (( #23658 ) ) ;
#5308 = B_SPLINE_CURVE_WITH_KNOTS ( 'NONE', 3,
 ( #1844, #5484, #66, #17935, #1386, #19737, #10715, #7416, #12436 ),
 .UNSPECIFIED., .F., .F.,
 ( 4, 2, 1, 2, 4 ),
 ( 6.245710625686469831E-20, 0.002165063509461098365, 0.004330127018922195863, 0.006495190528383293360, 0.008660254037844389990 ),
 .UNSPECIFIED. ) ;
#5309 = AXIS2_PLACEMENT_3D ( 'NONE', #3111, #17848, #4692 ) ;
#5310 = CIRCLE ( 'NONE', #4141, 2.199999999999979750 ) ;
#5311 = AXIS2_PLACEMENT_3D ( 'NONE', #2417, #18954, #17048 ) ;
#5312 = CARTESIAN_POINT ( 'NONE',  ( 119.9257125005558606, -1087.686723660049893, 30.00000000000641975 ) ) ;
#5313 = AXIS2_PLACEMENT_3D ( 'NONE', #6856, #2980, #3220 ) ;
#5314 = CARTESIAN_POINT ( 'NONE',  ( 50.00000000000000000, 5.616230220889763424E-16, -4.171999999999999709 ) ) ;
#5315 = VERTEX_POINT ( 'NONE', #2686 ) ;
#5316 = DIRECTION ( 'NONE',  ( 1.000000000000000000, 0.000000000000000000, 0.000000000000000000 ) ) ;
#5317 = ORIENTED_EDGE ( 'NONE', *, *, #11065, .T. ) ;
#5318 = CYLINDRICAL_SURFACE ( 'NONE', #16023, 5.200000000000031264 ) ;
#5319 = ADVANCED_FACE ( 'NONE', ( #20546, #11415 ), #18726, .F. ) ;
#5320 = CIRCLE ( 'NONE', #20333, 5.249999999999962697 ) ;
#5321 = ORIENTED_EDGE ( 'NONE', *, *, #3617, .T. ) ;
#5322 = EDGE_CURVE ( 'NONE', #9373, #8692, #4244, .T. ) ;
#5323 = LINE ( 'NONE', #14520, #18495 ) ;
#5324 = AXIS2_PLACEMENT_3D ( 'NONE', #20521, #3972, #18700 ) ;
#5325 = AXIS2_PLACEMENT_3D ( 'NONE', #10960, #9126, #21793 ) ;
#5326 = CARTESIAN_POINT ( 'NONE',  ( -6.482064212728073649, -1024.200416217147222, 145.0000119999999697 ) ) ;
#5327 = CYLINDRICAL_SURFACE ( 'NONE', #4164, 25.00000000000000000 ) ;
#5328 = CARTESIAN_POINT ( 'NONE',  ( 126.7787238282401461, 77.44864885511553609, -29.99999999999356248 ) ) ;
#5329 = VECTOR ( 'NONE', #11835, 1000.000000000000000 ) ;
#5330 = EDGE_CURVE ( 'NONE', #1528, #7205, #6421, .T. ) ;
#5331 = EDGE_CURVE ( 'NONE', #21739, #12627, #10554, .T. ) ;
#5332 = LINE ( 'NONE', #8967, #13118 ) ;
#5333 = ORIENTED_EDGE ( 'NONE', *, *, #3872, .T. ) ;
#5334 = CARTESIAN_POINT ( 'NONE',  ( 146.0000000000001990, -210.0000000000003411, -27.94499999999356632 ) ) ;
#5335 = EDGE_CURVE ( 'NONE', #10559, #17412, #15731, .T. ) ;
#5337 = VERTEX_POINT ( 'NONE', #10300 ) ;
#5336 = ORIENTED_EDGE ( 'NONE', *, *, #9820, .F. ) ;
#5338 = DIRECTION ( 'NONE',  ( 1.000000000000000000, -3.495664435217746987E-15, 0.000000000000000000 ) ) ;
#5339 = DIRECTION ( 'NONE',  ( 1.000000000000000000, 0.000000000000000000, 0.000000000000000000 ) ) ;
#5340 = CARTESIAN_POINT ( 'NONE',  ( -135.7895026000614678, -1074.740959209980247, 27.50000000000646239 ) ) ;
#5341 = ORIENTED_EDGE ( 'NONE', *, *, #16797, .T. ) ;
#5342 = PRESENTATION_LAYER_ASSIGNMENT (  '', '', ( #21973 ) ) ;
#5343 = DIRECTION ( 'NONE',  ( 0.000000000000000000, 0.000000000000000000, -1.000000000000000000 ) ) ;
#5344 = AXIS2_PLACEMENT_3D ( 'NONE', #19132, #22771, #11702 ) ;
#5345 = AXIS2_PLACEMENT_3D ( 'NONE', #10944, #21887, #5358 ) ;
#5346 = DIRECTION ( 'NONE',  ( 0.000000000000000000, 0.000000000000000000, 1.000000000000000000 ) ) ;
#5347 = CIRCLE ( 'NONE', #23073, 7.500000000000002665 ) ;
#5348 = VERTEX_POINT ( 'NONE', #19332 ) ;
#5349 = CARTESIAN_POINT ( 'NONE',  ( -79.04925354955248906, 121.5574576620396812, -90.00000000000000000 ) ) ;
#5350 = CARTESIAN_POINT ( 'NONE',  ( -24.99999999999998934, 45.00100000000031031, 34.99999999999983658 ) ) ;
#5351 = AXIS2_PLACEMENT_3D ( 'NONE', #23010, #6478, #19385 ) ;
#5352 = ORIENTED_EDGE ( 'NONE', *, *, #23144, .T. ) ;
#5353 = ORIENTED_EDGE ( 'NONE', *, *, #2358, .T. ) ;
#5354 = CARTESIAN_POINT ( 'NONE',  ( 125.7666110541943709, -1090.596734011949138, 31.26048023074375237 ) ) ;
#5355 = ORIENTED_EDGE ( 'NONE', *, *, #11732, .F. ) ;
#5356 = CARTESIAN_POINT ( 'NONE',  ( -280.2494876630257750, 272.8327955282141488, 146.3518577254344279 ) ) ;
#5357 = CARTESIAN_POINT ( 'NONE',  ( -160.0000000000000000, 0.000000000000000000, 100.0000000000000000 ) ) ;
#5358 = DIRECTION ( 'NONE',  ( 0.000000000000000000, -1.000000000000000000, 0.000000000000000000 ) ) ;
#5359 = PRODUCT ( 'motor mounting flange', 'motor mounting flange', '', ( #14852 ) ) ;
#5360 = AXIS2_PLACEMENT_3D ( 'NONE', #1717, #23700, #21776 ) ;
#5361 = DIRECTION ( 'NONE',  ( 0.000000000000000000, 0.000000000000000000, 1.000000000000000000 ) ) ;
#5362 = ADVANCED_FACE ( 'NONE', ( #8353 ), #23199, .T. ) ;
#5363 = EDGE_CURVE ( 'NONE', #885, #15690, #17732, .T. ) ;
#5364 = VECTOR ( 'NONE', #1722, 1000.000000000000114 ) ;
#5365 = AXIS2_PLACEMENT_3D ( 'NONE', #12085, #8536, #21325 ) ;
#5366 = CARTESIAN_POINT ( 'NONE',  ( 279.9999999999999432, 269.9999999999999432, 145.0000000000000284 ) ) ;
#5367 = ADVANCED_FACE ( 'NONE', ( #14061 ), #12257, .T. ) ;
#5368 = CIRCLE ( 'NONE', #18842, 145.0000000000000284 ) ;
#5369 = CIRCLE ( 'NONE', #360, 2.499999999999998668 ) ;
#5370 = CIRCLE ( 'NONE', #21941, 2.041999999999999815 ) ;
#5371 = ORIENTED_EDGE ( 'NONE', *, *, #12478, .T. ) ;
#5372 = DIRECTION ( 'NONE',  ( 0.000000000000000000, 0.000000000000000000, 1.000000000000000000 ) ) ;
#5373 = CARTESIAN_POINT ( 'NONE',  ( -7.500000000000000000, 0.7513028741560130452, -0.02472015219302865774 ) ) ;
#5374 = CARTESIAN_POINT ( 'NONE',  ( 107.6499999999999631, 35.00000000000000000, 0.000000000000000000 ) ) ;
#5375 = ORIENTED_EDGE ( 'NONE', *, *, #2311, .F. ) ;
#5376 = CARTESIAN_POINT ( 'NONE',  ( 110.0000000000000000, -74.99999999999998579, 0.000000000000000000 ) ) ;
#5377 = DIRECTION ( 'NONE',  ( -0.000000000000000000, 1.000000000000000000, 0.000000000000000000 ) ) ;
#5378 = CARTESIAN_POINT ( 'NONE',  ( -281.8958543268122980, 268.8927021017106540, 145.9952621458756425 ) ) ;
#5380 = AXIS2_PLACEMENT_3D ( 'NONE', #5183, #14152, #4948 ) ;
#5379 = AXIS2_PLACEMENT_3D ( 'NONE', #22129, #5372, #12792 ) ;
#5381 = CARTESIAN_POINT ( 'NONE',  ( -72.64999999999996305, -87.33333333333338544, 148.0000000000000000 ) ) ;
#5382 = AXIS2_PLACEMENT_3D ( 'NONE', #14177, #15428, #12622 ) ;
#5383 = DIRECTION ( 'NONE',  ( -0.000000000000000000, -0.000000000000000000, 1.000000000000000000 ) ) ;
#5384 = VECTOR ( 'NONE', #900, 1000.000000000000000 ) ;
#5385 = AXIS2_PLACEMENT_3D ( 'NONE', #19975, #20318, #3433 ) ;
#5386 = VERTEX_POINT ( 'NONE', #2791 ) ;
#5387 = AXIS2_PLACEMENT_3D ( 'NONE', #21794, #11321, #1853 ) ;
#5388 = VECTOR ( 'NONE', #9750, 1000.000000000000000 ) ;
#5389 = CARTESIAN_POINT ( 'NONE',  ( -312.2000000000014666, -132.2000000000000455, -146.4928932188134070 ) ) ;
#5390 = VERTEX_POINT ( 'NONE', #15619 ) ;
#5391 = CARTESIAN_POINT ( 'NONE',  ( 2.500000000000000000, -1.178949249685213863, 2.042000000000001148 ) ) ;
#5392 = CARTESIAN_POINT ( 'NONE',  ( 285.2000000000008981, 9.892604858775018348E-13, -146.4928932188134070 ) ) ;
#5393 = ORIENTED_EDGE ( 'NONE', *, *, #16362, .T. ) ;
#5394 = LINE ( 'NONE', #9377, #11545 ) ;
#5395 = DIRECTION ( 'NONE',  ( 0.000000000000000000, -1.000000000000000000, 0.000000000000000000 ) ) ;
#5396 = DIRECTION ( 'NONE',  ( -1.000000000000000000, -0.000000000000000000, -0.000000000000000000 ) ) ;
#5397 = DIRECTION ( 'NONE',  ( -1.000000000000000000, -0.000000000000000000, -0.000000000000000000 ) ) ;
#5398 = CARTESIAN_POINT ( 'NONE',  ( -281.4928932188135491, -129.2000000000000455, 152.4000000000014268 ) ) ;
#5399 = DIRECTION ( 'NONE',  ( 1.000000000000000000, 0.000000000000000000, 0.000000000000000000 ) ) ;
#5400 = CARTESIAN_POINT ( 'NONE',  ( -19.87769063953887283, 15.24974479720506437, 145.0000119999999981 ) ) ;
#5401 = VERTEX_POINT ( 'NONE', #23074 ) ;
#5402 = ORIENTED_EDGE ( 'NONE', *, *, #18682, .T. ) ;
#5404 = AXIS2_PLACEMENT_3D ( 'NONE', #2848, #16034, #17589 ) ;
#5403 = PRODUCT_DEFINITION_FORMATION_WITH_SPECIFIED_SOURCE ( 'ANY', '', #12925, .NOT_KNOWN. ) ;
#5405 = DIRECTION ( 'NONE',  ( 0.000000000000000000, 1.000000000000000000, 0.000000000000000000 ) ) ;
#5407 = CARTESIAN_POINT ( 'NONE',  ( 0.000000000000000000, 0.000000000000000000, -0.2800830152838844622 ) ) ;
#5406 =( REPRESENTATION_RELATIONSHIP ('NONE','NONE', #10127, #8987 ) REPRESENTATION_RELATIONSHIP_WITH_TRANSFORMATION ( #7153 )SHAPE_REPRESENTATION_RELATIONSHIP( ) );
#5408 =( GEOMETRIC_REPRESENTATION_CONTEXT ( 3 ) GLOBAL_UNCERTAINTY_ASSIGNED_CONTEXT ( ( #4320 ) ) GLOBAL_UNIT_ASSIGNED_CONTEXT ( ( #2444, #15390, #13612 ) ) REPRESENTATION_CONTEXT ( 'NONE', 'WORKASPACE' ) );
#5409 = AXIS2_PLACEMENT_3D ( 'NONE', #11677, #4013, #18984 ) ;
#5410 = ORIENTED_EDGE ( 'NONE', *, *, #23493, .T. ) ;
#5411 = AXIS2_PLACEMENT_3D ( 'NONE', #8487, #1101, #2898 ) ;
#5412 = CIRCLE ( 'NONE', #23135, 2.041999999999999815 ) ;
#5413 = CYLINDRICAL_SURFACE ( 'NONE', #17381, 2.649999999999985700 ) ;
#5414 = CARTESIAN_POINT ( 'NONE',  ( 1.500000000000000000, 12.00000000000000000, -50.00000000000000000 ) ) ;
#5415 = ORIENTED_EDGE ( 'NONE', *, *, #19779, .F. ) ;
#5416 = CARTESIAN_POINT ( 'NONE',  ( 281.4928932188133217, 267.7999999999999545, 147.1999999999999886 ) ) ;
#5417 = FACE_OUTER_BOUND ( 'NONE', #23397, .T. ) ;
#5418 = VERTEX_POINT ( 'NONE', #6549 ) ;
#5419 = CARTESIAN_POINT ( 'NONE',  ( -20.63749999999999574, 2.877919977996280320E-15, 23.50000000000000000 ) ) ;
#5420 = EDGE_LOOP ( 'NONE', ( #118, #23693, #15514, #9819, #2731 ) ) ;
#5421 = CARTESIAN_POINT ( 'NONE',  ( 7.549006887134069643, 4.358421158401191597, -7.700127545397312367 ) ) ;
#5422 = CARTESIAN_POINT ( 'NONE',  ( -136.9913212208047923, -1072.514673757700621, 30.16266818053254539 ) ) ;
#5423 = AXIS2_PLACEMENT_3D ( 'NONE', #14429, #14899, #22009 ) ;
#5424 = DIRECTION ( 'NONE',  ( 0.000000000000000000, -0.4999999999999993894, 0.8660254037844389297 ) ) ;
#5425 = ORIENTED_EDGE ( 'NONE', *, *, #5592, .T. ) ;
#5426 = EDGE_LOOP ( 'NONE', ( #10632, #3949 ) ) ;
#5427 = EDGE_CURVE ( 'NONE', #18124, #11437, #8411, .T. ) ;
#5428 = DIRECTION ( 'NONE',  ( 0.000000000000000000, 1.000000000000000000, -1.103561164596346103E-15 ) ) ;
#5429 = CIRCLE ( 'NONE', #13565, 4.057500000000000107 ) ;
#5430 = AXIS2_PLACEMENT_3D ( 'NONE', #23089, #8257, #19455 ) ;
#5431 = SHAPE_DEFINITION_REPRESENTATION ( #6890, #10127 ) ;
#5432 = CARTESIAN_POINT ( 'NONE',  ( 0.000000000000000000, 0.000000000000000000, 200.0000000000000000 ) ) ;
#5433 = CARTESIAN_POINT ( 'NONE',  ( 0.04606493828584144051, 9.175055303659556571, -8.057411785091790790 ) ) ;
#5434 = CARTESIAN_POINT ( 'NONE',  ( 45.00000000000002132, -56.79999999999935056, 140.0000000000001990 ) ) ;
#5435 = ADVANCED_FACE ( 'NONE', ( #13959 ), #3023, .F. ) ;
#5436 = ORIENTED_EDGE ( 'NONE', *, *, #17441, .T. ) ;
#5437 = DIRECTION ( 'NONE',  ( 0.000000000000000000, 0.000000000000000000, 1.000000000000000000 ) ) ;
#5438 = ADVANCED_FACE ( 'NONE', ( #21280 ), #3150, .F. ) ;
#5439 = EDGE_CURVE ( 'NONE', #12527, #22261, #23133, .T. ) ;
#5440 = DIRECTION ( 'NONE',  ( -1.000000000000000000, -0.000000000000000000, -0.000000000000000000 ) ) ;
#5441 = DIRECTION ( 'NONE',  ( 1.000000000000000000, 0.000000000000000000, 0.000000000000000000 ) ) ;
#5442 = VERTEX_POINT ( 'NONE', #10437 ) ;
#5443 = CARTESIAN_POINT ( 'NONE',  ( 1.013163106016871096, 8.075304045852551127, -7.231838333420561149 ) ) ;
#5444 = ORIENTED_EDGE ( 'NONE', *, *, #4005, .T. ) ;
#5445 = DIRECTION ( 'NONE',  ( 1.000000000000000000, 0.000000000000000000, 0.000000000000000000 ) ) ;
#5446 = CARTESIAN_POINT ( 'NONE',  ( -3.453038570459499024, -2.625189405340453419, -3.535263753545272891 ) ) ;
#5447 = EDGE_LOOP ( 'NONE', ( #18996, #8728, #7045, #14544 ) ) ;
#5448 = CARTESIAN_POINT ( 'NONE',  ( 0.000000000000000000, -127.0000000000000568, -150.2000000000013245 ) ) ;
#5449 = CARTESIAN_POINT ( 'NONE',  ( -22.47082401081929959, -1011.078780159199823, 145.0000119999999981 ) ) ;
#5450 = FACE_OUTER_BOUND ( 'NONE', #6468, .T. ) ;
#5451 = CARTESIAN_POINT ( 'NONE',  ( 125.3881179880844741, -1091.120112697373543, -27.99555145635498477 ) ) ;
#5452 = EDGE_CURVE ( 'NONE', #2405, #1528, #17783, .T. ) ;
#5453 = CARTESIAN_POINT ( 'NONE',  ( 2.687328764639642653, -3.067272167851299969, -0.05923475698271395140 ) ) ;
#5454 = ORIENTED_EDGE ( 'NONE', *, *, #8587, .T. ) ;
#5455 = CARTESIAN_POINT ( 'NONE',  ( -281.4928932188135491, -127.0000000000000568, 150.2000000000013813 ) ) ;
#5456 = PRODUCT_DEFINITION_SHAPE ( 'NONE', 'NONE',  #23885 ) ;
#5458 = ORIENTED_EDGE ( 'NONE', *, *, #12931, .F. ) ;
#5457 = EDGE_LOOP ( 'NONE', ( #8212, #20052, #4669 ) ) ;
#5459 = CARTESIAN_POINT ( 'NONE',  ( -277.2000000000006708, 90.00000000000096634, 34.99999999999999289 ) ) ;
#5460 = CYLINDRICAL_SURFACE ( 'NONE', #21600, 23.97500000000000497 ) ;
#5461 = DIRECTION ( 'NONE',  ( 0.7071067811865320296, 8.659560562355062281E-17, 0.7071067811865631159 ) ) ;
#5462 = ADVANCED_FACE ( 'NONE', ( #8597 ), #23431, .T. ) ;
#5463 = ORIENTED_EDGE ( 'NONE', *, *, #14844, .T. ) ;
#5464 = ADVANCED_FACE ( 'NONE', ( #21505 ), #1339, .F. ) ;
#5465 = DIRECTION ( 'NONE',  ( 0.000000000000000000, 1.177509268541832635E-16, -1.000000000000000000 ) ) ;
#5466 = CYLINDRICAL_SURFACE ( 'NONE', #14579, 20.00000000000000000 ) ;
#5467 = EDGE_CURVE ( 'NONE', #3608, #14489, #10913, .T. ) ;
#5468 = ORIENTED_EDGE ( 'NONE', *, *, #10154, .T. ) ;
#5469 = CYLINDRICAL_SURFACE ( 'NONE', #21551, 2.649999999999971934 ) ;
#5470 = CARTESIAN_POINT ( 'NONE',  ( -146.0000000000000568, -204.4690652294807478, 32.05500000000641592 ) ) ;
#5471 = EDGE_CURVE ( 'NONE', #14489, #4595, #5323, .T. ) ;
#5472 = ORIENTED_EDGE ( 'NONE', *, *, #9405, .T. ) ;
#5473 = VERTEX_POINT ( 'NONE', #7242 ) ;
#5474 = CARTESIAN_POINT ( 'NONE',  ( 125.9168667296001729, -1090.387741168242428, 30.65375098132854959 ) ) ;
#5475 = ORIENTED_EDGE ( 'NONE', *, *, #7252, .T. ) ;
#5476 = CARTESIAN_POINT ( 'NONE',  ( 16.51654882469417629, -981.1612794305008265, -145.0000000000001421 ) ) ;
#5477 = LINE ( 'NONE', #12649, #20375 ) ;
#5478 = CARTESIAN_POINT ( 'NONE',  ( 4.000000000000000000, -2.471525695159793035, -3.686886880705770864 ) ) ;
#5479 = CARTESIAN_POINT ( 'NONE',  ( -100.0000000000000000, -1400.000000000000000, 124.9999999999998295 ) ) ;
#5480 = FACE_OUTER_BOUND ( 'NONE', #14359, .T. ) ;
#5481 = ORIENTED_EDGE ( 'NONE', *, *, #2601, .F. ) ;
#5482 = EDGE_CURVE ( 'NONE', #11930, #11372, #18883, .T. ) ;
#5483 = DIRECTION ( 'NONE',  ( 1.000000000000000000, 0.000000000000000000, 0.000000000000000000 ) ) ;
#5484 = CARTESIAN_POINT ( 'NONE',  ( 0.6249999999999994449, -8.299410119600885594, -7.298562697733110838 ) ) ;
#5485 = EDGE_LOOP ( 'NONE', ( #21783, #1830, #23423, #18020, #388 ) ) ;
#5486 = CARTESIAN_POINT ( 'NONE',  ( -7.703011046602857601E-15, -132.2000000000000455, 0.000000000000000000 ) ) ;
#5487 = DIRECTION ( 'NONE',  ( 0.000000000000000000, 0.000000000000000000, -1.000000000000000000 ) ) ;
#5488 = EDGE_CURVE ( 'NONE', #1314, #10702, #3730, .T. ) ;
#5489 = CIRCLE ( 'NONE', #2001, 7.500000000000002665 ) ;
#5490 = CARTESIAN_POINT ( 'NONE',  ( -283.2140793454688605, 271.9822575857424454, 145.6220388411722695 ) ) ;
#5491 = ADVANCED_FACE ( 'NONE', ( #12969 ), #1804, .F. ) ;
#5492 = LINE ( 'NONE', #8910, #19581 ) ;
#5493 = EDGE_CURVE ( 'NONE', #7859, #13380, #7311, .T. ) ;
#5494 = DIRECTION ( 'NONE',  ( 0.000000000000000000, 1.000000000000000000, -1.287488025362403787E-15 ) ) ;
#5495 = ORIENTED_EDGE ( 'NONE', *, *, #6369, .T. ) ;
#5496 = CARTESIAN_POINT ( 'NONE',  ( -18.83467029480909360, -983.4793312354817090, 145.0000119999999697 ) ) ;
#5497 = ORIENTED_EDGE ( 'NONE', *, *, #4181, .T. ) ;
#5498 = CARTESIAN_POINT ( 'NONE',  ( 0.000000000000000000, 0.000000000000000000, -4.694516984716113228 ) ) ;
#5499 = CARTESIAN_POINT ( 'NONE',  ( 51.87806360044628917, 135.4018704341563080, -2.775557561562891351E-14 ) ) ;
#5500 = EDGE_LOOP ( 'NONE', ( #707, #10192 ) ) ;
#5501 = CARTESIAN_POINT ( 'NONE',  ( 153.5653415408401941, -1122.352966361446079, -27.49999999999322498 ) ) ;
#5502 = FACE_OUTER_BOUND ( 'NONE', #10010, .T. ) ;
#5503 = DIRECTION ( 'NONE',  ( 0.000000000000000000, -1.000000000000000000, -3.495664435217746987E-15 ) ) ;
#5504 = CARTESIAN_POINT ( 'NONE',  ( 24.99999999999998224, -1000.000000000000000, -145.0000060000000417 ) ) ;
#5505 = CARTESIAN_POINT ( 'NONE',  ( -7.703920929261752981, 4.447860822324863683, -7.917989418073281271 ) ) ;
#5506 = CARTESIAN_POINT ( 'NONE',  ( 0.000000000000000000, 0.000000000000000000, -50.00000000000000000 ) ) ;
#5507 = CARTESIAN_POINT ( 'NONE',  ( 22.47082401081929248, 11.07878015919987824, 145.0000119999999697 ) ) ;
#5508 = AXIS2_PLACEMENT_3D ( 'NONE', #4830, #12121, #1078 ) ;
#5509 = EDGE_LOOP ( 'NONE', ( #9912, #9444, #8670, #2860 ) ) ;
#5510 = VERTEX_POINT ( 'NONE', #13088 ) ;
#5511 = DIRECTION ( 'NONE',  ( 0.000000000000000000, 0.000000000000000000, 1.000000000000000000 ) ) ;
#5512 = CARTESIAN_POINT ( 'NONE',  ( -24.99999999999999645, 9.326071307568738836E-16, -145.0000059999999849 ) ) ;
#5513 = VERTEX_POINT ( 'NONE', #11148 ) ;
#5514 = EDGE_CURVE ( 'NONE', #13453, #19560, #18478, .T. ) ;
#5515 = DIRECTION ( 'NONE',  ( -0.000000000000000000, -0.000000000000000000, 1.000000000000000000 ) ) ;
#5516 = DIRECTION ( 'NONE',  ( 1.000000000000000000, 0.000000000000000000, 0.000000000000000000 ) ) ;
#5517 = ORIENTED_EDGE ( 'NONE', *, *, #4417, .F. ) ;
#5518 = CARTESIAN_POINT ( 'NONE',  ( 280.8708543776410806, 270.9956429438695409, 149.1582675804705218 ) ) ;
#5519 = DIRECTION ( 'NONE',  ( 0.000000000000000000, 0.000000000000000000, -1.000000000000000000 ) ) ;
#5520 = AXIS2_PLACEMENT_3D ( 'NONE', #15763, #8386, #11695 ) ;
#5521 = ORIENTED_EDGE ( 'NONE', *, *, #7371, .T. ) ;
#5522 = EDGE_CURVE ( 'NONE', #11363, #13630, #21979, .T. ) ;
#5523 = DIRECTION ( 'NONE',  ( -1.000000000000000000, 1.408839003528726857E-14, 6.982962677686266711E-15 ) ) ;
#5524 = CARTESIAN_POINT ( 'NONE',  ( -4.000000000000000000, 0.1981133338132459731, 2.096406544454392723E-17 ) ) ;
#5525 = CIRCLE ( 'NONE', #22852, 20.30000000000000071 ) ;
#5526 =( REPRESENTATION_RELATIONSHIP ('NONE','NONE', #10127, #18083 ) REPRESENTATION_RELATIONSHIP_WITH_TRANSFORMATION ( #11562 )SHAPE_REPRESENTATION_RELATIONSHIP( ) );
#5527 = LINE ( 'NONE', #20362, #8093 ) ;
#5528 = ORIENTED_EDGE ( 'NONE', *, *, #17271, .T. ) ;
#5529 = ADVANCED_FACE ( 'NONE', ( #23670 ), #22086, .F. ) ;
#5530 = CARTESIAN_POINT ( 'NONE',  ( 7.500000000000000888, 4.330127018922190985, -7.564338275809340928 ) ) ;
#5531 = CARTESIAN_POINT ( 'NONE',  ( -136.1788113199116310, -1074.029417785592614, 27.62610291900644555 ) ) ;
#5532 = ORIENTED_EDGE ( 'NONE', *, *, #16218, .F. ) ;
#5533 = ORIENTED_EDGE ( 'NONE', *, *, #9323, .F. ) ;
#5534 = DIRECTION ( 'NONE',  ( 1.000000000000000000, 0.000000000000000000, 0.000000000000000000 ) ) ;
#5535 = APPLICATION_PROTOCOL_DEFINITION ( 'draft international standard', 'automotive_design', 1998, #14786 ) ;
#5536 = DIRECTION ( 'NONE',  ( 1.000000000000000000, 0.000000000000000000, 0.000000000000000000 ) ) ;
#5537 = CARTESIAN_POINT ( 'NONE',  ( -44.99999999999997868, -59.79999999999935767, 197.6500000000001762 ) ) ;
#5538 = CYLINDRICAL_SURFACE ( 'NONE', #19375, 155.0000000000000284 ) ;
#5539 = AXIS2_PLACEMENT_3D ( 'NONE', #10156, #17498, #6752 ) ;
#5540 = VECTOR ( 'NONE', #11579, 1000.000000000000000 ) ;
#5541 = EDGE_LOOP ( 'NONE', ( #2116, #16606, #13467, #12615, #16349, #9301 ) ) ;
#5542 = CARTESIAN_POINT ( 'NONE',  ( -18.83467029480909005, -16.52066876451828037, 145.0000119999999697 ) ) ;
#5543 = B_SPLINE_CURVE_WITH_KNOTS ( 'NONE', 3,
 ( #7005, #9172, #16308, #21729, #9305, #22184, #3707, #18222, #14393, #10897, #16529, #23651, #14497, #21956, #12599, #19910, #1671, #5186, #7460, #5302, #21832, #7358, #9054, #22071, #8950, #11125, #16656, #12714, #16418, #14737, #111, #14610 ),
 .UNSPECIFIED., .F., .F.,
 ( 4, 2, 2, 2, 2, 2, 2, 2, 2, 2, 2, 2, 2, 2, 2, 4 ),
 ( 0.000000000000000000, 0.0004914281572963812407, 0.0009828563145927624815, 0.001474284471889143831, 0.001965712629185524963, 0.002457140786481906095, 0.002948568943778287661, 0.003931425258371062936, 0.004422853415667445803, 0.004914281572963828670, 0.005405709730260211537, 0.005897137887556594404, 0.006388566044852978139, 0.006879994202149361006, 0.007371422359445743873, 0.007862850516742125873 ),
 .UNSPECIFIED. ) ;
#5544 = UNCERTAINTY_MEASURE_WITH_UNIT (LENGTH_MEASURE( 1.000000000000000082E-05 ), #10344, 'distance_accuracy_value', 'NONE');
#5545 = ORIENTED_EDGE ( 'NONE', *, *, #20225, .F. ) ;
#5546 = CARTESIAN_POINT ( 'NONE',  ( -280.0000000000000568, 267.7999999999999545, -150.1999999999999318 ) ) ;
#5547 = CARTESIAN_POINT ( 'NONE',  ( 2.500000000000000000, 0.000000000000000000, 0.000000000000000000 ) ) ;
#5548 = ORIENTED_EDGE ( 'NONE', *, *, #5129, .F. ) ;
#5549 = CARTESIAN_POINT ( 'NONE',  ( 2.818872373871549124E-16, 8.716839668575678601, -7.700121441565840996 ) ) ;
#5550 = EDGE_CURVE ( 'NONE', #23104, #2171, #6164, .T. ) ;
#5551 = AXIS2_PLACEMENT_3D ( 'NONE', #11444, #12648, #5743 ) ;
#5552 = ORIENTED_EDGE ( 'NONE', *, *, #12743, .T. ) ;
#5553 = PRODUCT_DEFINITION_SHAPE ( 'NONE', 'NONE',  #16409 ) ;
#5554 = AXIS2_PLACEMENT_3D ( 'NONE', #2826, #796, #4527 ) ;
#5555 = DIRECTION ( 'NONE',  ( 0.000000000000000000, 0.000000000000000000, -1.000000000000000000 ) ) ;
#5556 = LINE ( 'NONE', #20273, #17489 ) ;
#5557 = VERTEX_POINT ( 'NONE', #20276 ) ;
#5558 = AXIS2_PLACEMENT_3D ( 'NONE', #5312, #9312, #18228 ) ;
#5559 = CARTESIAN_POINT ( 'NONE',  ( -129.1735827702798929, 85.66907061909597587, -28.88328940716463222 ) ) ;
#5560 = DIRECTION ( 'NONE',  ( -0.000000000000000000, 1.000000000000000000, -0.000000000000000000 ) ) ;
#5561 = CARTESIAN_POINT ( 'NONE',  ( -100.0000000000000000, -1400.000000000000000, -125.0000000000001705 ) ) ;
#5562 = CARTESIAN_POINT ( 'NONE',  ( 284.2295083325149108, 270.8299054689547347, 145.9020829022174439 ) ) ;
#5563 = CARTESIAN_POINT ( 'NONE',  ( 125.8126197883818520, -1090.532805371500899, -28.88328940716465354 ) ) ;
#5564 = CARTESIAN_POINT ( 'NONE',  ( 0.000000000000000000, 0.000000000000000000, -90.00000000000000000 ) ) ;
#5565 = ORIENTED_EDGE ( 'NONE', *, *, #22745, .F. ) ;
#5566 = DIRECTION ( 'NONE',  ( -0.7232617928448825673, 0.6905739489807055653, 6.982962677686266711E-15 ) ) ;
#5567 = FACE_OUTER_BOUND ( 'NONE', #1695, .T. ) ;
#5568 = AXIS2_PLACEMENT_3D ( 'NONE', #7317, #11572, #16487 ) ;
#5570 = ORIENTED_EDGE ( 'NONE', *, *, #1479, .F. ) ;
#5569 = ORIENTED_EDGE ( 'NONE', *, *, #6770, .F. ) ;
#5571 = CONICAL_SURFACE ( 'NONE', #20993, 2.055000000000000160, 0.7853981633974794763 ) ;
#5572 = DIRECTION ( 'NONE',  ( 0.000000000000000000, 0.000000000000000000, 1.000000000000000000 ) ) ;
#5573 = CARTESIAN_POINT ( 'NONE',  ( -136.6968504244152030, -1073.068359172758846, -28.34359615383088737 ) ) ;
#5574 = CARTESIAN_POINT ( 'NONE',  ( 281.2440776823445390, 268.3758453455904487, -147.1427398886702349 ) ) ;
#5575 = EDGE_LOOP ( 'NONE', ( #23599, #7158, #7140, #20153 ) ) ;
#5576 = CIRCLE ( 'NONE', #22925, 5.200000000000028599 ) ;
#5577 = CARTESIAN_POINT ( 'NONE',  ( 0.000000000000000000, -127.0000000000000568, 150.2000000000013813 ) ) ;
#5578 = ORIENTED_EDGE ( 'NONE', *, *, #12380, .T. ) ;
#5579 = EDGE_CURVE ( 'NONE', #6553, #21767, #1691, .T. ) ;
#5580 = DIRECTION ( 'NONE',  ( 0.000000000000000000, -1.000000000000000000, -1.110223024625156540E-16 ) ) ;
#5581 = EDGE_LOOP ( 'NONE', ( #21984, #3246 ) ) ;
#5582 = EDGE_CURVE ( 'NONE', #1647, #9091, #12744, .T. ) ;
#5583 = CARTESIAN_POINT ( 'NONE',  ( -79.99999999999995737, -56.80000000000003979, 5.199999999999971756 ) ) ;
#5584 = EDGE_CURVE ( 'NONE', #12385, #5390, #9074, .T. ) ;
#5585 = CONTEXT_DEPENDENT_SHAPE_REPRESENTATION ( #7405, #17403 ) ;
#5586 = ORIENTED_EDGE ( 'NONE', *, *, #21071, .F. ) ;
#5587 = SHAPE_REPRESENTATION ( 'hex flange nut gradea_iso_ISO - 4161 - M5 - N', ( #11210 ), #13515 ) ;
#5588 = CIRCLE ( 'NONE', #19073, 7.500000000000002665 ) ;
#5589 = CARTESIAN_POINT ( 'NONE',  ( 2.500000000000002220, 1.178949249685212086, -2.042000000000002036 ) ) ;
#5590 = ORIENTED_EDGE ( 'NONE', *, *, #4005, .F. ) ;
#5591 = CARTESIAN_POINT ( 'NONE',  ( -280.6228333615952693, 271.9320353020572156, 148.1755088701073930 ) ) ;
#5592 = EDGE_CURVE ( 'NONE', #2171, #22539, #16216, .T. ) ;
#5593 = ADVANCED_FACE ( 'NONE', ( #14409 ), #21853, .F. ) ;
#5594 = CARTESIAN_POINT ( 'NONE',  ( 133.4124711242726846, 78.90586732742401921, 27.75040112528346015 ) ) ;
#5595 = DIRECTION ( 'NONE',  ( 0.000000000000000000, 0.000000000000000000, -1.000000000000000000 ) ) ;
#5596 = CARTESIAN_POINT ( 'NONE',  ( -67.34999999999996589, -112.6666666666667140, 144.9999999999999716 ) ) ;
#5597 = DIRECTION ( 'NONE',  ( -0.000000000000000000, -0.000000000000000000, 1.000000000000000000 ) ) ;
#5598 = EDGE_LOOP ( 'NONE', ( #2561, #5131 ) ) ;
#5599 = EDGE_CURVE ( 'NONE', #16083, #4595, #12619, .T. ) ;
#5600 = CARTESIAN_POINT ( 'NONE',  ( -7.327471962526033167E-12, -994.4690652294825668, 0.000000000000000000 ) ) ;
#5601 = DIRECTION ( 'NONE',  ( 0.000000000000000000, -1.000000000000000000, 0.000000000000000000 ) ) ;
#5602 = AXIS2_PLACEMENT_3D ( 'NONE', #9765, #7705, #17121 ) ;
#5603 = CARTESIAN_POINT ( 'NONE',  ( -1.500000000000000000, 11.99999999999999822, 150.0000000000000284 ) ) ;
#5604 = ORIENTED_EDGE ( 'NONE', *, *, #171, .T. ) ;
#5605 = CARTESIAN_POINT ( 'NONE',  ( -44.99999999999995026, -56.79999999999968452, 105.0000000000002132 ) ) ;
#5606 = DIRECTION ( 'NONE',  ( 1.000000000000000000, -0.000000000000000000, -0.000000000000000000 ) ) ;
#5607 = DIRECTION ( 'NONE',  ( 0.000000000000000000, 0.000000000000000000, -1.000000000000000000 ) ) ;
#5608 = AXIS2_PLACEMENT_3D ( 'NONE', #15593, #21480, #19666 ) ;
#5609 = AXIS2_PLACEMENT_3D ( 'NONE', #6745, #8320, #13920 ) ;
#5610 = CARTESIAN_POINT ( 'NONE',  ( -67.34999999999996589, -87.33333333333338544, 124.9999999999999858 ) ) ;
#5611 = CARTESIAN_POINT ( 'NONE',  ( -312.2000000000014666, -129.2000000000000455, -146.4928932188134070 ) ) ;
#5612 = ORIENTED_EDGE ( 'NONE', *, *, #7257, .F. ) ;
#5613 = DIRECTION ( 'NONE',  ( 0.000000000000000000, 0.000000000000000000, 1.000000000000000000 ) ) ;
#5614 = VERTEX_POINT ( 'NONE', #5209 ) ;
#5615 =( NAMED_UNIT ( * ) SI_UNIT ( $, .STERADIAN. ) SOLID_ANGLE_UNIT ( ) );
#5616 = AXIS2_PLACEMENT_3D ( 'NONE', #3321, #17949, #18067 ) ;
#5617 = CARTESIAN_POINT ( 'NONE',  ( 0.000000000000000000, -1.178949249685213863, 2.042000000000002924 ) ) ;
#5618 = EDGE_CURVE ( 'NONE', #11437, #160, #3223, .T. ) ;
#5619 = EDGE_LOOP ( 'NONE', ( #4983, #9747, #9965, #961 ) ) ;
#5620 = SURFACE_SIDE_STYLE ('',( #18191 ) ) ;
#5621 = B_SPLINE_CURVE_WITH_KNOTS ( 'NONE', 3,
 ( #19529, #6993, #1196, #14485, #18209, #20013 ),
 .UNSPECIFIED., .F., .F.,
 ( 4, 2, 4 ),
 ( 2.475503369212747145E-07, 0.002222330217055634109, 0.004444412883774346255 ),
 .UNSPECIFIED. ) ;
#5622 = CARTESIAN_POINT ( 'NONE',  ( 123.4696136271386706, -1093.703085459773547, -31.88829724122655662 ) ) ;
#5623 = ADVANCED_FACE ( 'NONE', ( #20894 ), #13933, .F. ) ;
#5624 = DIRECTION ( 'NONE',  ( -1.350636282998972974E-14, 0.000000000000000000, -1.000000000000000000 ) ) ;
#5625 = CARTESIAN_POINT ( 'NONE',  ( 2.500000000000000000, 2.357898499370433054, -1.951563910473907981E-15 ) ) ;
#5626 = ADVANCED_FACE ( 'NONE', ( #495 ), #20759, .F. ) ;
#5627 = DIRECTION ( 'NONE',  ( 0.000000000000000000, 0.000000000000000000, 1.000000000000000000 ) ) ;
#5628 = CARTESIAN_POINT ( 'NONE',  ( -287.4000000000014552, -127.0000000000000568, 146.4928932188134638 ) ) ;
#5629 = DIRECTION ( 'NONE',  ( -1.000000000000000000, 7.709882115452476934E-17, 0.000000000000000000 ) ) ;
#5630 = AXIS2_PLACEMENT_3D ( 'NONE', #22862, #6093, #4401 ) ;
#5631 = EDGE_CURVE ( 'NONE', #21515, #2402, #19067, .T. ) ;
#5632 = ORIENTED_EDGE ( 'NONE', *, *, #22787, .T. ) ;
#5633 = EDGE_CURVE ( 'NONE', #8807, #17283, #2531, .T. ) ;
#5634 = EDGE_LOOP ( 'NONE', ( #5548, #20199 ) ) ;
#5635 = DIRECTION ( 'NONE',  ( 0.000000000000000000, 0.000000000000000000, 1.000000000000000000 ) ) ;
#5636 = LINE ( 'NONE', #14376, #15059 ) ;
#5637 = ADVANCED_FACE ( 'NONE', ( #7974 ), #9687, .T. ) ;
#5638 = ORIENTED_EDGE ( 'NONE', *, *, #13754, .F. ) ;
#5639 = CARTESIAN_POINT ( 'NONE',  ( 5.000000000000000000, 4.685197434473814759, -5.637851296924623057E-15 ) ) ;
#5640 = CARTESIAN_POINT ( 'NONE',  ( 6.439685834477092641, -4.942299687812566233, -7.659344964963564983 ) ) ;
#5641 = AXIS2_PLACEMENT_3D ( 'NONE', #17200, #4278, #11431 ) ;
#5642 = DIRECTION ( 'NONE',  ( 0.000000000000000000, -1.000000000000000000, -4.694093751100962712E-16 ) ) ;
#5643 = EDGE_LOOP ( 'NONE', ( #6395, #18496 ) ) ;
#5644 = DIRECTION ( 'NONE',  ( 0.000000000000000000, 0.000000000000000000, -1.000000000000000000 ) ) ;
#5645 = CARTESIAN_POINT ( 'NONE',  ( 2.699999999999997513, 0.000000000000000000, 0.000000000000000000 ) ) ;
#5646 = CARTESIAN_POINT ( 'NONE',  ( 5.036189803708990276, -8.737863883542580368, 200.0000119999999981 ) ) ;
#5647 = ORIENTED_EDGE ( 'NONE', *, *, #20190, .T. ) ;
#5648 = DIRECTION ( 'NONE',  ( -0.000000000000000000, -0.000000000000000000, 1.000000000000000000 ) ) ;
#5649 = DIRECTION ( 'NONE',  ( 1.000000000000000000, -0.000000000000000000, -0.000000000000000000 ) ) ;
#5650 = CARTESIAN_POINT ( 'NONE',  ( 0.000000000000000000, 0.000000000000000000, 100.0000000000000000 ) ) ;
#5651 = VERTEX_POINT ( 'NONE', #13692 ) ;
#5652 = CARTESIAN_POINT ( 'NONE',  ( 281.3689414351989626, 272.8938770989752811, -145.2488155364688680 ) ) ;
#5653 = PRODUCT_CONTEXT ( 'NONE', #20475, 'mechanical' ) ;
#5654 = PLANE ( 'NONE',  #5804 ) ;
#5655 = CIRCLE ( 'NONE', #13018, 2.649999999999971934 ) ;
#5656 = FACE_OUTER_BOUND ( 'NONE', #17417, .T. ) ;
#5657 = CARTESIAN_POINT ( 'NONE',  ( 281.2440776823444253, 268.3758453455903918, 147.1427398886702917 ) ) ;
#5658 = LINE ( 'NONE', #13070, #21701 ) ;
#5659 = VERTEX_POINT ( 'NONE', #22568 ) ;
#5660 = ORIENTED_EDGE ( 'NONE', *, *, #14325, .T. ) ;
#5661 = EDGE_CURVE ( 'NONE', #21513, #6476, #11502, .T. ) ;
#5662 = CARTESIAN_POINT ( 'NONE',  ( -6.482064212728082531, -24.20041621714725011, 145.0000119999999697 ) ) ;
#5663 = EDGE_CURVE ( 'NONE', #5111, #10051, #8112, .T. ) ;
#5664 = PRODUCT_DEFINITION_CONTEXT ( 'detailed design', #7209, 'design' ) ;
#5665 = VECTOR ( 'NONE', #19072, 1000.000000000000114 ) ;
#5666 = ORIENTED_EDGE ( 'NONE', *, *, #8394, .F. ) ;
#5667 = DIRECTION ( 'NONE',  ( 0.000000000000000000, -0.000000000000000000, 1.000000000000000000 ) ) ;
#5668 = LINE ( 'NONE', #9421, #6827 ) ;
#5669 = VERTEX_POINT ( 'NONE', #2293 ) ;
#5670 = CIRCLE ( 'NONE', #23794, 2.199999999999979750 ) ;
#5671 = CARTESIAN_POINT ( 'NONE',  ( -145.0000000000000284, 0.000000000000000000, -90.00000000000000000 ) ) ;
#5672 = ORIENTED_EDGE ( 'NONE', *, *, #15086, .T. ) ;
#5673 = SURFACE_SIDE_STYLE ('',( #17034 ) ) ;
#5674 = DIRECTION ( 'NONE',  ( -1.110223024625155594E-14, 0.000000000000000000, -1.000000000000000000 ) ) ;
#5675 = EDGE_LOOP ( 'NONE', ( #3318, #9562, #8182, #2909 ) ) ;
#5676 = DIRECTION ( 'NONE',  ( -1.000000000000000000, 0.000000000000000000, 0.000000000000000000 ) ) ;
#5677 = DIRECTION ( 'NONE',  ( -1.000000000000000000, -0.000000000000000000, -0.000000000000000000 ) ) ;
#5678 = PLANE ( 'NONE',  #7075 ) ;
#5679 = CIRCLE ( 'NONE', #22248, 0.3000000000000016542 ) ;
#5680 = CARTESIAN_POINT ( 'NONE',  ( 284.1268706878666990, 270.9682701916306087, 145.8706349181169628 ) ) ;
#5681 = FACE_OUTER_BOUND ( 'NONE', #14860, .T. ) ;
#5682 = CARTESIAN_POINT ( 'NONE',  ( -93.00000000000000000, 3.000000000000308198, 129.9038105676659711 ) ) ;
#5683 = ORIENTED_EDGE ( 'NONE', *, *, #10708, .T. ) ;
#5684 = CARTESIAN_POINT ( 'NONE',  ( -24.99999999999995381, -52.79999999999965610, 65.00000000000018474 ) ) ;
#5685 = AXIS2_PLACEMENT_3D ( 'NONE', #8743, #21055, #4512 ) ;
#5686 = CARTESIAN_POINT ( 'NONE',  ( -24.99999999999998224, -52.79999999999944293, 125.0000000000001990 ) ) ;
#5687 = FILL_AREA_STYLE_COLOUR ( '', #17365 ) ;
#5688 = AXIS2_PLACEMENT_3D ( 'NONE', #11158, #8729, #14763 ) ;
#5689 = CIRCLE ( 'NONE', #20733, 0.3000000000000051514 ) ;
#5691 = EDGE_LOOP ( 'NONE', ( #14828, #9992 ) ) ;
#5690 = ORIENTED_EDGE ( 'NONE', *, *, #8316, .T. ) ;
#5692 = DIRECTION ( 'NONE',  ( 0.000000000000000000, 0.000000000000000000, 1.000000000000000000 ) ) ;
#5693 = DIRECTION ( 'NONE',  ( -1.000000000000000000, -0.000000000000000000, -0.000000000000000000 ) ) ;
#5694 = CARTESIAN_POINT ( 'NONE',  ( 280.2488155364688396, 272.8938770989753948, -146.3689414351990195 ) ) ;
#5695 = EDGE_LOOP ( 'NONE', ( #20282, #23163 ) ) ;
#5696 = CARTESIAN_POINT ( 'NONE',  ( -134.5479913728701717, -1076.953479568426701, 29.67150201188731984 ) ) ;
#5697 = VERTEX_POINT ( 'NONE', #11643 ) ;
#5698 = VECTOR ( 'NONE', #22282, 1000.000000000000000 ) ;
#5699 = CARTESIAN_POINT ( 'NONE',  ( 284.1320353020572611, 270.9755088701073191, -145.8700598572183651 ) ) ;
#5700 = ORIENTED_EDGE ( 'NONE', *, *, #17469, .T. ) ;
#5701 = DIRECTION ( 'NONE',  ( -3.700743415417187942E-15, 1.000000000000000000, 0.000000000000000000 ) ) ;
#5702 = DIRECTION ( 'NONE',  ( 0.000000000000000000, 0.000000000000000000, -1.000000000000000000 ) ) ;
#5703 = CONTEXT_DEPENDENT_SHAPE_REPRESENTATION ( #18960, #10279 ) ;
#5704 = EDGE_LOOP ( 'NONE', ( #7763, #9804, #14728, #19769 ) ) ;
#5705 = DIRECTION ( 'NONE',  ( 0.000000000000000000, -1.000000000000000000, 0.000000000000000000 ) ) ;
#5706 = ORIENTED_EDGE ( 'NONE', *, *, #613, .T. ) ;
#5707 =( REPRESENTATION_RELATIONSHIP ('NONE','NONE', #10127, #5587 ) REPRESENTATION_RELATIONSHIP_WITH_TRANSFORMATION ( #13239 )SHAPE_REPRESENTATION_RELATIONSHIP( ) );
#5708 = CARTESIAN_POINT ( 'NONE',  ( -64.99999999999997158, -56.79999999999975557, 35.00000000000019185 ) ) ;
#5709 = DIRECTION ( 'NONE',  ( 0.000000000000000000, 0.000000000000000000, 1.000000000000000000 ) ) ;
#5710 = ADVANCED_FACE ( 'NONE', ( #13444 ), #247, .F. ) ;
#5711 = CARTESIAN_POINT ( 'NONE',  ( -146.0000000000004832, -784.4690652294799520, -27.94499999999356632 ) ) ;
#5712 = FACE_OUTER_BOUND ( 'NONE', #5288, .T. ) ;
#5713 = CARTESIAN_POINT ( 'NONE',  ( -281.2440776823445390, 269.1610889986682764, -150.0646579186752092 ) ) ;
#5714 = FACE_OUTER_BOUND ( 'NONE', #7928, .T. ) ;
#5715 = ORIENTED_EDGE ( 'NONE', *, *, #2170, .T. ) ;
#5716 = ADVANCED_FACE ( 'NONE', ( #17154, #16909 ), #6168, .T. ) ;
#5717 = DIRECTION ( 'NONE',  ( 1.000000000000000000, 0.000000000000000000, 0.000000000000000000 ) ) ;
#5718 = VECTOR ( 'NONE', #2043, 1000.000000000000000 ) ;
#5719 = CARTESIAN_POINT ( 'NONE',  ( 26.98333333333330231, -89.99999999999998579, 3.000000000000000000 ) ) ;
#5720 = VECTOR ( 'NONE', #17826, 1000.000000000000000 ) ;
#5721 = DIRECTION ( 'NONE',  ( -1.000000000000000000, 0.000000000000000000, 0.000000000000000000 ) ) ;
#5722 = EDGE_CURVE ( 'NONE', #12103, #321, #9664, .T. ) ;
#5723 = AXIS2_PLACEMENT_3D ( 'NONE', #6012, #2018, #7461 ) ;
#5724 = CIRCLE ( 'NONE', #6882, 2.041999999999999815 ) ;
#5725 = CARTESIAN_POINT ( 'NONE',  ( 281.0927021017106426, 269.6958543268121957, 145.4976310729378497 ) ) ;
#5726 = FACE_OUTER_BOUND ( 'NONE', #9930, .T. ) ;
#5727 = EDGE_CURVE ( 'NONE', #20258, #19773, #4629, .T. ) ;
#5728 = CIRCLE ( 'NONE', #6507, 23.50000000000000000 ) ;
#5729 =( BOUNDED_SURFACE ( )  B_SPLINE_SURFACE ( 3, 2, ( 
 ( #3727, #9193, #9072 ),
 ( #1253, #5446, #15998 ),
 ( #5007, #23103, #21983 ),
 ( #3607, #14635, #16434 ),
 ( #10330, #3172, #13981 ),
 ( #12170, #21304, #11026 ) ),
 .UNSPECIFIED., .F., .F., .F. ) 
 B_SPLINE_SURFACE_WITH_KNOTS ( ( 4, 2, 4 ),
 ( 3, 3 ),
 ( 0.02032853247518126918, 0.02278863295364821906, 0.02524873343211516893 ),
 ( 0.000000000000000000, 1.000000000000000000 ),
 .UNSPECIFIED. ) 
 GEOMETRIC_REPRESENTATION_ITEM ( )  RATIONAL_B_SPLINE_SURFACE ( (
 ( 1.000000000000000000, 0.8047781615896838492, 1.000000000000000000),
 ( 1.000000000000000000, 0.8123767586288186404, 1.000000000000000000),
 ( 1.000000000000000000, 0.8190662415565814758, 1.000000000000000000),
 ( 1.000000000000000000, 0.8192361015667604107, 1.000000000000000000),
 ( 1.000000000000000000, 0.8126135807104967190, 1.000000000000000000),
 ( 1.000000000000000000, 0.8047712338318580017, 1.000000000000000000) ) ) 
 REPRESENTATION_ITEM ( '' )  SURFACE ( )  );
#5730 = DIRECTION ( 'NONE',  ( -0.000000000000000000, -0.000000000000000000, 1.000000000000000000 ) ) ;
#5731 = FACE_OUTER_BOUND ( 'NONE', #18854, .T. ) ;
#5732 = ITEM_DEFINED_TRANSFORMATION ( 'NONE', 'NONE', #12756,  #11210 ) ;
#5733 = ORIENTED_EDGE ( 'NONE', *, *, #2270, .F. ) ;
#5734 = CARTESIAN_POINT ( 'NONE',  ( 3.272451888078286686, -975.1611521969856540, 145.0000119999999981 ) ) ;
#5735 = EDGE_LOOP ( 'NONE', ( #24, #22433, #19438, #15105 ) ) ;
#5737 = CARTESIAN_POINT ( 'NONE',  ( -52.99999999999997158, -56.80000000000003268, 5.199999999999971756 ) ) ;
#5736 = CIRCLE ( 'NONE', #4199, 2.041999999999999815 ) ;
#5738 = FILL_AREA_STYLE_COLOUR ( '', #8707 ) ;
#5740 = AXIS2_PLACEMENT_3D ( 'NONE', #9744, #4036, #17098 ) ;
#5739 = STYLED_ITEM ( 'NONE', ( #7983 ), #9029 ) ;
#5741 = AXIS2_PLACEMENT_3D ( 'NONE', #21707, #23271, #15365 ) ;
#5742 = CIRCLE ( 'NONE', #9221, 35.00000000000000711 ) ;
#5743 = DIRECTION ( 'NONE',  ( 0.000000000000000000, -1.000000000000000000, 0.000000000000000000 ) ) ;
#5744 = VECTOR ( 'NONE', #6375, 1000.000000000000114 ) ;
#5745 = ORIENTED_EDGE ( 'NONE', *, *, #20222, .F. ) ;
#5746 = DIRECTION ( 'NONE',  ( 1.110223024625157172E-14, 0.000000000000000000, -1.000000000000000000 ) ) ;
#5747 = VECTOR ( 'NONE', #1105, 1000.000000000000000 ) ;
#5748 = CARTESIAN_POINT ( 'NONE',  ( 2.500000000000002220, 3.469446951953614189E-15, 2.041999999999998483 ) ) ;
#5749 = DIRECTION ( 'NONE',  ( -1.000000000000000000, 1.408839003528726857E-14, 6.982962677686266711E-15 ) ) ;
#5750 = DIRECTION ( 'NONE',  ( 1.000000000000000000, -0.000000000000000000, 6.982962677686266711E-15 ) ) ;
#5751 = DIRECTION ( 'NONE',  ( 1.000000000000000000, 0.000000000000000000, 0.000000000000000000 ) ) ;
#5752 = DIRECTION ( 'NONE',  ( 0.000000000000000000, 0.000000000000000000, -1.000000000000000000 ) ) ;
#5753 = AXIS2_PLACEMENT_3D ( 'NONE', #17540, #989, #12411 ) ;
#5754 = CARTESIAN_POINT ( 'NONE',  ( -7.499999999999653610, -1.545780083834116247, -7.491787297939224821 ) ) ;
#5755 = ORIENTED_EDGE ( 'NONE', *, *, #18667, .F. ) ;
#5756 = SURFACE_SIDE_STYLE ('',( #15605 ) ) ;
#5757 = CARTESIAN_POINT ( 'NONE',  ( -44.99999999999997868, -52.79999999999936477, 195.0000000000001705 ) ) ;
#5758 = DIRECTION ( 'NONE',  ( -0.000000000000000000, -0.000000000000000000, 1.000000000000000000 ) ) ;
#5759 = ORIENTED_EDGE ( 'NONE', *, *, #14624, .T. ) ;
#5760 = ADVANCED_FACE ( 'NONE', ( #2041 ), #9432, .F. ) ;
#5761 = AXIS2_PLACEMENT_3D ( 'NONE', #16711, #5709, #15386 ) ;
#5762 = CYLINDRICAL_SURFACE ( 'NONE', #8124, 35.00000000000000711 ) ;
#5763 = CARTESIAN_POINT ( 'NONE',  ( 100.0000000000000000, -1420.000000000000000, -145.0000000000001705 ) ) ;
#5764 = CIRCLE ( 'NONE', #19246, 45.00000000000000711 ) ;
#5765 = AXIS2_PLACEMENT_3D ( 'NONE', #2850, #19158, #15573 ) ;
#5766 = EDGE_CURVE ( 'NONE', #3355, #2544, #17057, .T. ) ;
#5767 = VECTOR ( 'NONE', #8891, 1000.000000000000000 ) ;
#5768 = AXIS2_PLACEMENT_3D ( 'NONE', #13586, #2534, #15358 ) ;
#5769 = CARTESIAN_POINT ( 'NONE',  ( -285.2000000000000455, 267.7999999999999545, 0.000000000000000000 ) ) ;
#5770 = CIRCLE ( 'NONE', #21574, 21.50000000000000000 ) ;
#5771 = AXIS2_PLACEMENT_3D ( 'NONE', #7346, #14727, #3712 ) ;
#5772 = EDGE_CURVE ( 'NONE', #7386, #8023, #12119, .T. ) ;
#5773 = ORIENTED_EDGE ( 'NONE', *, *, #14805, .F. ) ;
#5774 = CARTESIAN_POINT ( 'NONE',  ( -20.63749999999999574, 0.000000000000000000, 0.000000000000000000 ) ) ;
#5775 = CARTESIAN_POINT ( 'NONE',  ( 0.000000000000000000, 0.000000000000000000, 200.0000119999999981 ) ) ;
#5776 = ADVANCED_FACE ( 'NONE', ( #19541 ), #1163, .F. ) ;
#5777 = DIRECTION ( 'NONE',  ( 1.110223024625157172E-14, 0.000000000000000000, -1.000000000000000000 ) ) ;
#5778 = ORIENTED_EDGE ( 'NONE', *, *, #7182, .T. ) ;
#5779 = DIRECTION ( 'NONE',  ( 1.000000000000000000, 0.000000000000000000, 0.000000000000000000 ) ) ;
#5781 = CARTESIAN_POINT ( 'NONE',  ( 1.118033988749894458, 0.000000000000000000, 0.000000000000000000 ) ) ;
#5780 = PRODUCT_DEFINITION ( 'UNKNOWN', '', #2709, #11485 ) ;
#5782 = DIRECTION ( 'NONE',  ( 0.000000000000000000, 0.000000000000000000, -1.000000000000000000 ) ) ;
#5783 = EDGE_LOOP ( 'NONE', ( #9715, #9854, #19988, #21303 ) ) ;
#5784 = DIRECTION ( 'NONE',  ( -1.000000000000000000, -0.000000000000000000, -0.000000000000000000 ) ) ;
#5785 = PRODUCT_CONTEXT ( 'NONE', #1505, 'mechanical' ) ;
#5786 = CARTESIAN_POINT ( 'NONE',  ( 3.000000000000002665, 0.000000000000000000, -24.69999999999999929 ) ) ;
#5788 = AXIS2_PLACEMENT_3D ( 'NONE', #2718, #8270, #1003 ) ;
#5787 = AXIS2_PLACEMENT_3D ( 'NONE', #5600, #19342, #2566 ) ;
#5790 = FACE_BOUND ( 'NONE', #22978, .T. ) ;
#5789 = PRESENTATION_LAYER_ASSIGNMENT (  '', '', ( #1542 ) ) ;
#5791 = VECTOR ( 'NONE', #13227, 1000.000000000000000 ) ;
#5792 = FACE_OUTER_BOUND ( 'NONE', #5485, .T. ) ;
#5793 = VECTOR ( 'NONE', #23523, 1000.000000000000000 ) ;
#5794 = ORIENTED_EDGE ( 'NONE', *, *, #14090, .T. ) ;
#5795 = VERTEX_POINT ( 'NONE', #4828 ) ;
#5796 = CARTESIAN_POINT ( 'NONE',  ( 0.000000000000000000, 0.000000000000000000, -4.484454397937119197 ) ) ;
#5797 = FACE_OUTER_BOUND ( 'NONE', #19410, .T. ) ;
#5798 = AXIS2_PLACEMENT_3D ( 'NONE', #8303, #22894, #21093 ) ;
#5799 = DIRECTION ( 'NONE',  ( -1.000000000000000000, 1.408839003528726857E-14, 6.982962677686266711E-15 ) ) ;
#5800 = DIRECTION ( 'NONE',  ( 0.000000000000000000, 0.000000000000000000, 1.000000000000000000 ) ) ;
#5801 = AXIS2_PLACEMENT_3D ( 'NONE', #3878, #1594, #16335 ) ;
#5802 = ORIENTED_EDGE ( 'NONE', *, *, #7660, .T. ) ;
#5803 = LINE ( 'NONE', #22683, #22575 ) ;
#5804 = AXIS2_PLACEMENT_3D ( 'NONE', #16882, #3947, #18926 ) ;
#5805 = AXIS2_PLACEMENT_3D ( 'NONE', #9994, #11828, #19373 ) ;
#5806 = EDGE_LOOP ( 'NONE', ( #20737, #15392 ) ) ;
#5807 = EDGE_CURVE ( 'NONE', #22213, #11691, #15841, .T. ) ;
#5808 = DIRECTION ( 'NONE',  ( 0.000000000000000000, 0.000000000000000000, -1.000000000000000000 ) ) ;
#5809 = ADVANCED_FACE ( 'NONE', ( #8578 ), #12236, .F. ) ;
#5810 = DIRECTION ( 'NONE',  ( 0.000000000000000000, 1.177509268541832635E-16, -1.000000000000000000 ) ) ;
#5811 = ORIENTED_EDGE ( 'NONE', *, *, #23434, .F. ) ;
#5812 = CARTESIAN_POINT ( 'NONE',  ( -128.0869692137157188, 87.28547799715830990, -27.51562286569268068 ) ) ;
#5813 = CARTESIAN_POINT ( 'NONE',  ( -280.0000000000000568, 272.9999999999999432, -144.9999999999999716 ) ) ;
#5814 = CARTESIAN_POINT ( 'NONE',  ( -12.52876685377501786, -1021.695789975588468, 145.0000119999999981 ) ) ;
#5815 = CARTESIAN_POINT ( 'NONE',  ( -281.1045205713626842, 269.7080393212557965, -145.4986342070536978 ) ) ;
#5816 = CARTESIAN_POINT ( 'NONE',  ( -3.750000000000004885, 6.495190528383289141, 0.000000000000000000 ) ) ;
#5817 = LINE ( 'NONE', #22345, #6126 ) ;
#5818 = VERTEX_POINT ( 'NONE', #1316 ) ;
#5819 = ORIENTED_EDGE ( 'NONE', *, *, #7398, .T. ) ;
#5820 = DIRECTION ( 'NONE',  ( 0.000000000000000000, 0.000000000000000000, -1.000000000000000000 ) ) ;
#5821 = DIRECTION ( 'NONE',  ( 0.000000000000000000, 0.000000000000000000, -1.000000000000000000 ) ) ;
#5823 = ORIENTED_EDGE ( 'NONE', *, *, #10769, .T. ) ;
#5822 = EDGE_LOOP ( 'NONE', ( #16592, #12037, #16861, #8360, #9617, #19551, #1308, #3794 ) ) ;
#5824 = DIRECTION ( 'NONE',  ( -0.7071067811865416886, 9.961996129952529179E-15, -0.7071067811865532349 ) ) ;
#5825 = DIRECTION ( 'NONE',  ( 1.000000000000000000, 0.000000000000000000, 0.000000000000000000 ) ) ;
#5826 = ORIENTED_EDGE ( 'NONE', *, *, #11717, .F. ) ;
#5827 = ORIENTED_EDGE ( 'NONE', *, *, #3694, .F. ) ;
#5828 = DIRECTION ( 'NONE',  ( 0.000000000000000000, 0.000000000000000000, 1.000000000000000000 ) ) ;
#5829 = ORIENTED_EDGE ( 'NONE', *, *, #185, .T. ) ;
#5830 = EDGE_CURVE ( 'NONE', #9561, #21081, #10405, .T. ) ;
#5831 = FACE_OUTER_BOUND ( 'NONE', #15927, .T. ) ;
#5832 = CARTESIAN_POINT ( 'NONE',  ( -40.00000000000000000, 100.0000000000000000, 150.2000000000009550 ) ) ;
#5833 = ORIENTED_EDGE ( 'NONE', *, *, #17205, .F. ) ;
#5834 = ADVANCED_FACE ( 'NONE', ( #6398 ), #23046, .T. ) ;
#5835 = DIRECTION ( 'NONE',  ( 0.000000000000000000, 0.000000000000000000, -1.000000000000000000 ) ) ;
#5836 = ORIENTED_EDGE ( 'NONE', *, *, #4634, .T. ) ;
#5837 = CARTESIAN_POINT ( 'NONE',  ( -280.1247002395581376, 272.9663407402831012, 145.6822561791009321 ) ) ;
#5838 = CARTESIAN_POINT ( 'NONE',  ( -1.747541505913277282, 3.837784562140256650, -3.503702292528906526 ) ) ;
#5839 = CARTESIAN_POINT ( 'NONE',  ( 45.00000000000002132, -52.79999999999933635, 197.6500000000002046 ) ) ;
#5840 = PLANE ( 'NONE',  #11770 ) ;
#5841 = ORIENTED_EDGE ( 'NONE', *, *, #8556, .T. ) ;
#5842 = CARTESIAN_POINT ( 'NONE',  ( -281.4928932188134354, 267.7999999999999545, -150.2299999999999329 ) ) ;
#5843 = ORIENTED_EDGE ( 'NONE', *, *, #16315, .F. ) ;
#5844 = DIRECTION ( 'NONE',  ( -1.000000000000000000, 0.000000000000000000, -6.982962677686266711E-15 ) ) ;
#5845 = DIRECTION ( 'NONE',  ( -1.000000000000000000, -0.000000000000000000, -0.000000000000000000 ) ) ;
#5846 = DIRECTION ( 'NONE',  ( -0.000000000000000000, -0.000000000000000000, 1.000000000000000000 ) ) ;
#5847 = CARTESIAN_POINT ( 'NONE',  ( 284.5699028110927316, 270.4339272673396977, 145.9952621458756710 ) ) ;
#5848 = CARTESIAN_POINT ( 'NONE',  ( 7.499999999999997335, 34.18698582794336005, 100.0000000000000000 ) ) ;
#5849 = EDGE_CURVE ( 'NONE', #6867, #15717, #14279, .T. ) ;
#5850 = ADVANCED_FACE ( 'NONE', ( #10280 ), #19676, .F. ) ;
#5851 = LINE ( 'NONE', #9486, #18664 ) ;
#5852 = CARTESIAN_POINT ( 'NONE',  ( 123.1514321905984417, -1094.120844545941964, 28.74044610054851745 ) ) ;
#5853 = ORIENTED_EDGE ( 'NONE', *, *, #1825, .T. ) ;
#5854 = DIRECTION ( 'NONE',  ( 1.000000000000000000, 0.000000000000000000, 0.000000000000000000 ) ) ;
#5855 = ORIENTED_EDGE ( 'NONE', *, *, #14840, .F. ) ;
#5856 = LINE ( 'NONE', #8033, #12328 ) ;
#5857 = PRESENTATION_STYLE_ASSIGNMENT (( #15063 ) ) ;
#5858 = DIRECTION ( 'NONE',  ( -0.9423651898111409242, -0.3345860861306287903, 6.982962677686267499E-15 ) ) ;
#5859 = ORIENTED_EDGE ( 'NONE', *, *, #7296, .F. ) ;
#5860 = DIRECTION ( 'NONE',  ( 1.000000000000000000, -0.000000000000000000, 6.982962677686266711E-15 ) ) ;
#5861 = DIRECTION ( 'NONE',  ( 0.000000000000000000, -2.618450529776326854E-15, -1.000000000000000000 ) ) ;
#5862 = DIRECTION ( 'NONE',  ( -1.000000000000000000, -0.000000000000000000, -0.000000000000000000 ) ) ;
#5863 = CARTESIAN_POINT ( 'NONE',  ( -2.100000000000000089, 2.571758278209441957E-16, -5.000000000000000000 ) ) ;
#5864 = CARTESIAN_POINT ( 'NONE',  ( 2.500000000000000000, -2.357898499370431722, 2.818925648462311528E-15 ) ) ;
#5865 = ADVANCED_FACE ( 'NONE', ( #15599 ), #21322, .F. ) ;
#5866 = CARTESIAN_POINT ( 'NONE',  ( -4.000000000000000000, -1.942223658245633811, -0.3516579909967644246 ) ) ;
#5867 = CARTESIAN_POINT ( 'NONE',  ( -7.915341292092594294, -3.857523022641989652, -7.913710289178173873 ) ) ;
#5868 = EDGE_LOOP ( 'NONE', ( #8382, #17611, #19900, #18241 ) ) ;
#5869 = CARTESIAN_POINT ( 'NONE',  ( -110.0000000000000000, 75.00000000000001421, 0.000000000000000000 ) ) ;
#5870 = DIRECTION ( 'NONE',  ( 1.000000000000000000, 3.736327486719276364E-16, 1.067522139062650425E-16 ) ) ;
#5871 = ORIENTED_EDGE ( 'NONE', *, *, #5885, .T. ) ;
#5872 = VECTOR ( 'NONE', #11716, 1000.000000000000000 ) ;
#5873 = EDGE_LOOP ( 'NONE', ( #6690, #5393 ) ) ;
#5874 = DIRECTION ( 'NONE',  ( 0.000000000000000000, 0.000000000000000000, 1.000000000000000000 ) ) ;
#5875 = DIRECTION ( 'NONE',  ( -1.000000000000000000, -0.000000000000000000, -0.000000000000000000 ) ) ;
#5876 = FACE_OUTER_BOUND ( 'NONE', #23483, .T. ) ;
#5877 = ORIENTED_EDGE ( 'NONE', *, *, #19695, .T. ) ;
#5878 = DIRECTION ( 'NONE',  ( 3.736327486719275871E-16, -1.000000000000000000, 3.469446951953613794E-15 ) ) ;
#5879 = CARTESIAN_POINT ( 'NONE',  ( -155.0000000000000284, -1000.000000000000000, 90.00000000000000000 ) ) ;
#5880 = DIRECTION ( 'NONE',  ( 0.8191520442889875797, 0.000000000000000000, 0.5735764363510522656 ) ) ;
#5881 = ORIENTED_EDGE ( 'NONE', *, *, #17201, .F. ) ;
#5882 = EDGE_CURVE ( 'NONE', #11264, #6579, #5543, .T. ) ;
#5883 = CARTESIAN_POINT ( 'NONE',  ( 281.0570750465942638, 270.1062614524586820, 149.6728700860325318 ) ) ;
#5884 = CARTESIAN_POINT ( 'NONE',  ( 65.00000000000001421, -52.79999999999938609, 125.0000000000002274 ) ) ;
#5885 = EDGE_CURVE ( 'NONE', #16800, #16453, #5429, .T. ) ;
#5886 = DIRECTION ( 'NONE',  ( 1.000000000000000000, 0.000000000000000000, 0.000000000000000000 ) ) ;
#5887 = EDGE_LOOP ( 'NONE', ( #274, #3648, #716, #11634 ) ) ;
#5888 = CARTESIAN_POINT ( 'NONE',  ( 281.0927021017106426, 269.6958543268121957, -145.4976310729377644 ) ) ;
#5889 = AXIS2_PLACEMENT_3D ( 'NONE', #3713, #10768, #3361 ) ;
#5890 = APPLICATION_PROTOCOL_DEFINITION ( 'draft international standard', 'automotive_design', 1998, #14346 ) ;
#5891 = FACE_BOUND ( 'NONE', #10859, .T. ) ;
#5892 = EDGE_CURVE ( 'NONE', #6350, #21582, #17770, .T. ) ;
#5893 = CARTESIAN_POINT ( 'NONE',  ( 235.0000000000000284, -499.9999999999999432, -56.99999999999997158 ) ) ;
#5894 = LINE ( 'NONE', #698, #17464 ) ;
#5895 = EDGE_CURVE ( 'NONE', #11791, #9794, #3359, .T. ) ;
#5896 = ORIENTED_EDGE ( 'NONE', *, *, #20806, .T. ) ;
#5897 = VERTEX_POINT ( 'NONE', #18443 ) ;
#5898 = DIRECTION ( 'NONE',  ( 0.000000000000000000, 0.000000000000000000, -1.000000000000000000 ) ) ;
#5899 = DIRECTION ( 'NONE',  ( -1.000000000000000000, -0.000000000000000000, -0.000000000000000000 ) ) ;
#5900 = PRODUCT_DEFINITION_CONTEXT ( 'detailed design', #23255, 'design' ) ;
#5901 = CIRCLE ( 'NONE', #2810, 5.249999999999973355 ) ;
#5902 = DIRECTION ( 'NONE',  ( -0.000000000000000000, 1.000000000000000000, -3.469446951953613794E-15 ) ) ;
#5903 = LINE ( 'NONE', #238, #10323 ) ;
#5904 = ORIENTED_EDGE ( 'NONE', *, *, #12596, .T. ) ;
#5905 = CARTESIAN_POINT ( 'NONE',  ( -285.2000000000012960, -74.99999999999899103, 90.00000000000000000 ) ) ;
#5906 = ORIENTED_EDGE ( 'NONE', *, *, #11282, .F. ) ;
#5907 = DIRECTION ( 'NONE',  ( -1.000000000000000000, -0.000000000000000000, -0.000000000000000000 ) ) ;
#5908 = LINE ( 'NONE', #4085, #12534 ) ;
#5909 = ORIENTED_EDGE ( 'NONE', *, *, #14633, .T. ) ;
#5910 = ORIENTED_EDGE ( 'NONE', *, *, #11723, .T. ) ;
#5911 = PLANE ( 'NONE',  #2694 ) ;
#5912 = AXIS2_PLACEMENT_3D ( 'NONE', #7907, #15293, #13510 ) ;
#5913 = CARTESIAN_POINT ( 'NONE',  ( -280.0627246244602020, 273.0000000000000568, -145.3431883566700549 ) ) ;
#5914 = AXIS2_PLACEMENT_3D ( 'NONE', #13960, #3265, #7023 ) ;
#5915 = ADVANCED_FACE ( 'NONE', ( #20144, #16189 ), #3590, .T. ) ;
#5916 = CARTESIAN_POINT ( 'NONE',  ( 70.00000000000000000, -112.6666666666666714, 3.000000000000000000 ) ) ;
#5917 = EDGE_CURVE ( 'NONE', #10526, #11121, #16600, .T. ) ;
#5918 = DIRECTION ( 'NONE',  ( -0.5000000000000051070, 0.000000000000000000, 0.8660254037844355990 ) ) ;
#5919 = CARTESIAN_POINT ( 'NONE',  ( -110.0000000000000000, 75.00000000000001421, 3.000000000000000000 ) ) ;
#5920 = DIRECTION ( 'NONE',  ( 1.000000000000000000, 0.000000000000000000, 0.000000000000000000 ) ) ;
#5921 = ADVANCED_FACE ( 'NONE', ( #18329 ), #1782, .F. ) ;
#5922 = CARTESIAN_POINT ( 'NONE',  ( -7.500000000000000000, -1.486698507076798847, -0.09861472150523968583 ) ) ;
#5923 = ORIENTED_EDGE ( 'NONE', *, *, #20310, .T. ) ;
#5924 = EDGE_CURVE ( 'NONE', #10981, #3142, #1565, .T. ) ;
#5925 = DIRECTION ( 'NONE',  ( -1.000000000000000000, -0.000000000000000000, -0.000000000000000000 ) ) ;
#5926 = CARTESIAN_POINT ( 'NONE',  ( -31.74999999999995737, 0.000000000000000000, 0.000000000000000000 ) ) ;
#5927 = SURFACE_STYLE_USAGE ( .BOTH. , #9558 ) ;
#5929 = EDGE_LOOP ( 'NONE', ( #3486, #3638 ) ) ;
#5928 = ORIENTED_EDGE ( 'NONE', *, *, #14515, .F. ) ;
#5930 = EDGE_CURVE ( 'NONE', #301, #10091, #1568, .T. ) ;
#5931 = CARTESIAN_POINT ( 'NONE',  ( -136.9835704417553757, -1072.529321614196760, -29.67081494451417001 ) ) ;
#5932 = CARTESIAN_POINT ( 'NONE',  ( 280.1244295015775378, 273.0299999999999727, -145.6847249064869061 ) ) ;
#5933 = EDGE_CURVE ( 'NONE', #23782, #14990, #416, .T. ) ;
#5934 = ORIENTED_EDGE ( 'NONE', *, *, #19297, .T. ) ;
#5935 = AXIS2_PLACEMENT_3D ( 'NONE', #7351, #1427, #12483 ) ;
#5936 = CARTESIAN_POINT ( 'NONE',  ( -135.2464651929976753, -1075.719328653694674, 27.75096515221176219 ) ) ;
#5937 = AXIS2_PLACEMENT_3D ( 'NONE', #16851, #5982, #9380 ) ;
#5938 = ORIENTED_EDGE ( 'NONE', *, *, #9057, .F. ) ;
#5939 = CARTESIAN_POINT ( 'NONE',  ( -20.63749999999999574, 0.000000000000000000, 0.000000000000000000 ) ) ;
#5940 = VERTEX_POINT ( 'NONE', #5786 ) ;
#5941 = DIRECTION ( 'NONE',  ( -1.000000000000000000, 0.000000000000000000, 0.000000000000000000 ) ) ;
#5942 = ORIENTED_EDGE ( 'NONE', *, *, #20073, .T. ) ;
#5943 = EDGE_CURVE ( 'NONE', #14308, #7318, #7712, .T. ) ;
#5944 = DIRECTION ( 'NONE',  ( 0.000000000000000000, 0.000000000000000000, -1.000000000000000000 ) ) ;
#5945 = ORIENTED_EDGE ( 'NONE', *, *, #19719, .T. ) ;
#5946 = CARTESIAN_POINT ( 'NONE',  ( -12.52399064350059277, -978.3009594173067853, -145.0000000000001137 ) ) ;
#5947 = SURFACE_SIDE_STYLE ('',( #16819 ) ) ;
#5948 = DIRECTION ( 'NONE',  ( -1.000000000000000000, -0.000000000000000000, -0.000000000000000000 ) ) ;
#5949 = COLOUR_RGB ( '',1.000000000000000000, 0.9490196078431372140, 0.9098039215686274384 ) ;
#5950 = AXIS2_PLACEMENT_3D ( 'NONE', #13132, #16713, #3898 ) ;
#5951 = CARTESIAN_POINT ( 'NONE',  ( -72.64999999999996305, -87.33333333333338544, 3.000000000000000000 ) ) ;
#5952 = EDGE_LOOP ( 'NONE', ( #20876, #11563 ) ) ;
#5953 = CARTESIAN_POINT ( 'NONE',  ( -280.0000000000000000, 273.0299999999999727, -144.9999999999999716 ) ) ;
#5954 =( NAMED_UNIT ( * ) PLANE_ANGLE_UNIT ( ) SI_UNIT ( $, .RADIAN. ) );
#5955 = AXIS2_PLACEMENT_3D ( 'NONE', #10633, #14381, #20241 ) ;
#5956 = ORIENTED_EDGE ( 'NONE', *, *, #20695, .T. ) ;
#5957 = DIRECTION ( 'NONE',  ( -6.580500949201930884E-15, -2.336402151923303105E-15, -1.000000000000000000 ) ) ;
#5958 = ADVANCED_FACE ( 'NONE', ( #2257, #474 ), #17020, .F. ) ;
#5959 = CARTESIAN_POINT ( 'NONE',  ( 281.4928932188134354, -127.0000000000000568, -152.4000000000012847 ) ) ;
#5960 = CARTESIAN_POINT ( 'NONE',  ( -7.499999999999999112, 41.99999999999998579, -100.0000000000000000 ) ) ;
#5961 = ADVANCED_FACE ( 'NONE', ( #20497 ), #5654, .F. ) ;
#5962 = CARTESIAN_POINT ( 'NONE',  ( 280.6807971656550080, 272.9999999999999432, 145.1244294735509470 ) ) ;
#5963 = CARTESIAN_POINT ( 'NONE',  ( -112.7436279071531828, 91.18044947428914782, -2.775557561562891351E-14 ) ) ;
#5964 = ORIENTED_EDGE ( 'NONE', *, *, #12059, .T. ) ;
#5965 = DIRECTION ( 'NONE',  ( 1.000000000000000000, 0.000000000000000000, 0.000000000000000000 ) ) ;
#5966 = AXIS2_PLACEMENT_3D ( 'NONE', #18997, #8031, #17332 ) ;
#5967 = DIRECTION ( 'NONE',  ( 0.000000000000000000, -1.000000000000000000, 0.000000000000000000 ) ) ;
#5968 = CARTESIAN_POINT ( 'NONE',  ( 123.1031131805789016, -1094.184009126530555, 28.88679084683406018 ) ) ;
#5969 = ITEM_DEFINED_TRANSFORMATION ( 'NONE', 'NONE', #759,  #11210 ) ;
#5970 = VERTEX_POINT ( 'NONE', #11357 ) ;
#5971 = DIRECTION ( 'NONE',  ( -1.350636282998972974E-14, 0.000000000000000000, -1.000000000000000000 ) ) ;
#5972 = ORIENTED_EDGE ( 'NONE', *, *, #15084, .F. ) ;
#5973 = VECTOR ( 'NONE', #8060, 1000.000000000000000 ) ;
#5974 = FACE_BOUND ( 'NONE', #12898, .T. ) ;
#5975 = DIRECTION ( 'NONE',  ( 1.000000000000000000, 0.000000000000000000, 0.000000000000000000 ) ) ;
#5976 = EDGE_LOOP ( 'NONE', ( #2140, #15894 ) ) ;
#5977 = DIRECTION ( 'NONE',  ( 1.000000000000000000, 0.000000000000000000, 0.000000000000000000 ) ) ;
#5978 = EDGE_LOOP ( 'NONE', ( #6753, #17830 ) ) ;
#5979 = DIRECTION ( 'NONE',  ( -1.000000000000000000, 0.000000000000000000, 0.000000000000000000 ) ) ;
#5980 = PLANE ( 'NONE',  #22662 ) ;
#5981 = CARTESIAN_POINT ( 'NONE',  ( 0.000000000000000000, 0.000000000000000000, 0.000000000000000000 ) ) ;
#5982 = DIRECTION ( 'NONE',  ( 3.202566417187928841E-16, -1.000000000000000000, 3.469446951953614583E-15 ) ) ;
#5983 = CARTESIAN_POINT ( 'NONE',  ( 0.000000000000000000, 0.000000000000000000, 0.000000000000000000 ) ) ;
#5984 = AXIS2_PLACEMENT_3D ( 'NONE', #2395, #20740, #6146 ) ;
#5985 = DIRECTION ( 'NONE',  ( 0.000000000000000000, 0.000000000000000000, 1.000000000000000000 ) ) ;
#5986 = DIRECTION ( 'NONE',  ( 3.495664435217746987E-15, -1.000000000000000000, 0.000000000000000000 ) ) ;
#5987 =( REPRESENTATION_RELATIONSHIP ('NONE','NONE', #10127, #18083 ) REPRESENTATION_RELATIONSHIP_WITH_TRANSFORMATION ( #2621 )SHAPE_REPRESENTATION_RELATIONSHIP( ) );
#5988 = CIRCLE ( 'NONE', #18685, 0.5155456020628804703 ) ;
#5989 = ORIENTED_EDGE ( 'NONE', *, *, #11895, .F. ) ;
#5990 = FACE_BOUND ( 'NONE', #8015, .T. ) ;
#5991 = LINE ( 'NONE', #20712, #10065 ) ;
#5992 = ORIENTED_EDGE ( 'NONE', *, *, #4998, .F. ) ;
#5993 = VECTOR ( 'NONE', #13266, 1000.000000000000000 ) ;
#5994 = ORIENTED_EDGE ( 'NONE', *, *, #10538, .T. ) ;
#5995 = PLANE ( 'NONE',  #15078 ) ;
#5996 = FACE_OUTER_BOUND ( 'NONE', #1396, .T. ) ;
#5997 = DIRECTION ( 'NONE',  ( 1.000000000000000000, 0.000000000000000000, 0.000000000000000000 ) ) ;
#5998 = ORIENTED_EDGE ( 'NONE', *, *, #8394, .T. ) ;
#5999 = AXIS2_PLACEMENT_3D ( 'NONE', #11082, #3449, #14460 ) ;
#6000 = CARTESIAN_POINT ( 'NONE',  ( 155.0000000000000284, -500.0000000000000000, 32.50000000000001421 ) ) ;
#6001 = CARTESIAN_POINT ( 'NONE',  ( 7.499999999999999112, 41.99999999999998579, 100.0000000000000000 ) ) ;
#6002 = CARTESIAN_POINT ( 'NONE',  ( -9.739726766683155290, -2.617478843592798921, 200.0000119999999981 ) ) ;
#6003 = EDGE_LOOP ( 'NONE', ( #12964, #1422, #2014, #19233 ) ) ;
#6004 = PLANE ( 'NONE',  #2124 ) ;
#6005 = AXIS2_PLACEMENT_3D ( 'NONE', #7369, #7235, #3499 ) ;
#6006 = DIRECTION ( 'NONE',  ( -1.000000000000000000, 0.000000000000000000, 0.000000000000000000 ) ) ;
#6007 = UNCERTAINTY_MEASURE_WITH_UNIT (LENGTH_MEASURE( 1.000000000000000082E-05 ), #12146, 'distance_accuracy_value', 'NONE');
#6008 = EDGE_LOOP ( 'NONE', ( #18302, #1200, #529, #10134 ) ) ;
#6009 = DIRECTION ( 'NONE',  ( 0.000000000000000000, 0.000000000000000000, 1.000000000000000000 ) ) ;
#6010 = AXIS2_PLACEMENT_3D ( 'NONE', #15147, #20796, #13353 ) ;
#6011 = CARTESIAN_POINT ( 'NONE',  ( 155.0000000000000568, -801.0618695410399823, 30.00000000000648015 ) ) ;
#6012 = CARTESIAN_POINT ( 'NONE',  ( -2.699999999999995737, 0.000000000000000000, 0.000000000000000000 ) ) ;
#6013 = CARTESIAN_POINT ( 'NONE',  ( 5.000000000000000000, 4.969004387540385421E-16, -4.057500000000000107 ) ) ;
#6014 = ORIENTED_EDGE ( 'NONE', *, *, #8841, .F. ) ;
#6015 = ORIENTED_EDGE ( 'NONE', *, *, #18351, .F. ) ;
#6016 = CARTESIAN_POINT ( 'NONE',  ( 155.0000000000000284, -500.0000000000000000, 30.00000000000001421 ) ) ;
#6017 = AXIS2_PLACEMENT_3D ( 'NONE', #22251, #14922, #3906 ) ;
#6018 = DIRECTION ( 'NONE',  ( -1.000000000000000000, 0.000000000000000000, 0.000000000000000000 ) ) ;
#6019 = EDGE_CURVE ( 'NONE', #20774, #9451, #10448, .T. ) ;
#6020 = EDGE_CURVE ( 'NONE', #13899, #1268, #8078, .T. ) ;
#6021 = ADVANCED_FACE ( 'NONE', ( #9659 ), #16764, .T. ) ;
#6022 = ORIENTED_EDGE ( 'NONE', *, *, #15684, .F. ) ;
#6023 = CARTESIAN_POINT ( 'NONE',  ( 100.0000000000000000, 269.9999999999999432, 125.0000000000000284 ) ) ;
#6024 = CARTESIAN_POINT ( 'NONE',  ( -288.2000000000013529, -89.99999999999896261, -40.33333333333332860 ) ) ;
#6025 = ORIENTED_EDGE ( 'NONE', *, *, #10406, .F. ) ;
#6026 = DIRECTION ( 'NONE',  ( 1.000000000000000000, 3.469446951953630952E-16, 4.625929269271474081E-16 ) ) ;
#6027 = ADVANCED_FACE ( 'NONE', ( #584, #5891, #11254, #18671, #11614, #7951, #20734, #15210, #4195, #13065 ), #15329, .T. ) ;
#6028 = EDGE_LOOP ( 'NONE', ( #514, #6048 ) ) ;
#6029 = DIRECTION ( 'NONE',  ( 0.000000000000000000, 0.000000000000000000, 1.000000000000000000 ) ) ;
#6030 = FACE_OUTER_BOUND ( 'NONE', #2993, .T. ) ;
#6031 = VERTEX_POINT ( 'NONE', #346 ) ;
#6032 = ORIENTED_EDGE ( 'NONE', *, *, #13492, .F. ) ;
#6033 = CARTESIAN_POINT ( 'NONE',  ( 232.0000000000000284, -490.0000000000000000, 9.066821367772113093E-13 ) ) ;
#6034 = DIRECTION ( 'NONE',  ( 1.000000000000000000, -0.000000000000000000, -0.000000000000000000 ) ) ;
#6035 = DIRECTION ( 'NONE',  ( 0.000000000000000000, -0.000000000000000000, 1.000000000000000000 ) ) ;
#6036 = CARTESIAN_POINT ( 'NONE',  ( 34.75000000000005684, 100.0000000000000000, 125.0000000000000000 ) ) ;
#6037 = DIRECTION ( 'NONE',  ( -0.000000000000000000, -0.000000000000000000, 1.000000000000000000 ) ) ;
#6038 = DIRECTION ( 'NONE',  ( 1.000000000000000000, -0.000000000000000000, -0.000000000000000000 ) ) ;
#6039 = LINE ( 'NONE', #15489, #9620 ) ;
#6040 = ORIENTED_EDGE ( 'NONE', *, *, #16103, .F. ) ;
#6041 = CARTESIAN_POINT ( 'NONE',  ( 279.9999999999999432, -127.0000000000000568, 147.2000000000013813 ) ) ;
#6042 = CARTESIAN_POINT ( 'NONE',  ( -7.847095227763516867, -4.129731495738496960, -7.493596212620239783 ) ) ;
#6043 = AXIS2_PLACEMENT_3D ( 'NONE', #6819, #16126, #9442 ) ;
#6044 = ORIENTED_EDGE ( 'NONE', *, *, #20262, .F. ) ;
#6045 = CARTESIAN_POINT ( 'NONE',  ( -282.2000000000007276, 75.00000000000099476, -90.00000000000000000 ) ) ;
#6046 = CIRCLE ( 'NONE', #10720, 145.0000000000000284 ) ;
#6047 = CARTESIAN_POINT ( 'NONE',  ( 281.3684665762324926, 268.0840560642351988, -147.1696999999999207 ) ) ;
#6048 = ORIENTED_EDGE ( 'NONE', *, *, #23000, .F. ) ;
#6049 = ADVANCED_FACE ( 'NONE', ( #2387 ), #19673, .T. ) ;
#6050 = CARTESIAN_POINT ( 'NONE',  ( -135.4738523116355964, -1075.311763300250277, 32.42126403526991396 ) ) ;
#6051 = ORIENTED_EDGE ( 'NONE', *, *, #3710, .F. ) ;
#6052 = CARTESIAN_POINT ( 'NONE',  ( 7.500000000000000000, -4.330127018922199866, -7.422398894150035176 ) ) ;
#6053 = EDGE_CURVE ( 'NONE', #8574, #4532, #13948, .T. ) ;
#6054 = CARTESIAN_POINT ( 'NONE',  ( 281.6795879751484222, 272.7329465209282375, -145.3118087683467934 ) ) ;
#6055 = EDGE_CURVE ( 'NONE', #6737, #4834, #3488, .T. ) ;
#6056 = EDGE_LOOP ( 'NONE', ( #1810, #7210 ) ) ;
#6057 = CARTESIAN_POINT ( 'NONE',  ( 146.0000000000002274, -799.0068695410406008, -29.99999999999356604 ) ) ;
#6058 =( NAMED_UNIT ( * ) PLANE_ANGLE_UNIT ( ) SI_UNIT ( $, .RADIAN. ) );
#6059 = AXIS2_PLACEMENT_3D ( 'NONE', #2858, #12105, #932 ) ;
#6060 = EDGE_LOOP ( 'NONE', ( #6871, #1089, #8119, #10717, #22180 ) ) ;
#6061 = EDGE_CURVE ( 'NONE', #2756, #679, #11236, .T. ) ;
#6062 = ADVANCED_FACE ( 'NONE', ( #4067 ), #18565, .T. ) ;
#6063 = CARTESIAN_POINT ( 'NONE',  ( 90.00000000000000000, -149.9999999999996874, 129.9038105676659711 ) ) ;
#6064 = VERTEX_POINT ( 'NONE', #22305 ) ;
#6065 = CARTESIAN_POINT ( 'NONE',  ( -6.487720809262722987, -975.8007591756590955, -145.0000000000001421 ) ) ;
#6066 = AXIS2_PLACEMENT_3D ( 'NONE', #18558, #7454, #2011 ) ;
#6067 = DIRECTION ( 'NONE',  ( 0.000000000000000000, -1.000000000000000000, 0.000000000000000000 ) ) ;
#6068 = CARTESIAN_POINT ( 'NONE',  ( -40.33333333333332860, -89.99999999999997158, 3.000000000000001332 ) ) ;
#6069 = DIRECTION ( 'NONE',  ( -1.000000000000000000, -0.000000000000000000, -0.000000000000000000 ) ) ;
#6070 = ORIENTED_EDGE ( 'NONE', *, *, #12779, .F. ) ;
#6071 = CARTESIAN_POINT ( 'NONE',  ( -282.1854425596108058, 268.0906609804448522, 146.3673129565597719 ) ) ;
#6072 = FILL_AREA_STYLE_COLOUR ( '', #19651 ) ;
#6074 = ORIENTED_EDGE ( 'NONE', *, *, #13128, .F. ) ;
#6073 = VERTEX_POINT ( 'NONE', #11477 ) ;
#6075 = DIRECTION ( 'NONE',  ( -0.9423651898111408132, -0.3345860861306287348, 0.000000000000000000 ) ) ;
#6076 = CYLINDRICAL_SURFACE ( 'NONE', #22755, 145.0000000000000284 ) ;
#6077 = DIRECTION ( 'NONE',  ( 0.000000000000000000, 0.000000000000000000, -1.000000000000000000 ) ) ;
#6078 = AXIS2_PLACEMENT_3D ( 'NONE', #7806, #19014, #17226 ) ;
#6079 = DIRECTION ( 'NONE',  ( 0.000000000000000000, 0.000000000000000000, -1.000000000000000000 ) ) ;
#6080 = CYLINDRICAL_SURFACE ( 'NONE', #6017, 7.500000000000007105 ) ;
#6081 = AXIS2_PLACEMENT_3D ( 'NONE', #16936, #403, #152 ) ;
#6082 = ORIENTED_EDGE ( 'NONE', *, *, #13829, .F. ) ;
#6083 = AXIS2_PLACEMENT_3D ( 'NONE', #21310, #2823, #1144 ) ;
#6084 = DIRECTION ( 'NONE',  ( -1.000000000000000000, 0.000000000000000000, 0.000000000000000000 ) ) ;
#6085 = CONICAL_SURFACE ( 'NONE', #4941, 2.055000000000001492, 0.7853981633974633780 ) ;
#6086 = CARTESIAN_POINT ( 'NONE',  ( -194.7500000000000284, -784.4690652294799520, 30.00000000000675726 ) ) ;
#6087 = CARTESIAN_POINT ( 'NONE',  ( 123.8014913250401037, -1093.264216588538829, 27.75040112528339975 ) ) ;
#6088 = ITEM_DEFINED_TRANSFORMATION ( 'NONE', 'NONE', #23107,  #11210 ) ;
#6089 = ORIENTED_EDGE ( 'NONE', *, *, #19223, .F. ) ;
#6090 = DIRECTION ( 'NONE',  ( 6.640089860198304064E-16, 1.000000000000000000, -4.183096374613631247E-18 ) ) ;
#6091 = ORIENTED_EDGE ( 'NONE', *, *, #21075, .F. ) ;
#6092 = CARTESIAN_POINT ( 'NONE',  ( 0.000000000000000000, 0.000000000000000000, -8.499999999999998224 ) ) ;
#6093 = DIRECTION ( 'NONE',  ( 0.000000000000000000, 0.000000000000000000, 1.000000000000000000 ) ) ;
#6094 = ADVANCED_FACE ( 'NONE', ( #18795 ), #6372, .F. ) ;
#6095 = EDGE_CURVE ( 'NONE', #22094, #18595, #10064, .T. ) ;
#6096 = ORIENTED_EDGE ( 'NONE', *, *, #17236, .F. ) ;
#6097 = EDGE_CURVE ( 'NONE', #22916, #15482, #12799, .T. ) ;
#6098 = DIRECTION ( 'NONE',  ( 1.000000000000000000, 0.000000000000000000, 0.000000000000000000 ) ) ;
#6099 = ORIENTED_EDGE ( 'NONE', *, *, #2102, .T. ) ;
#6100 = AXIS2_PLACEMENT_3D ( 'NONE', #20679, #11313, #18622 ) ;
#6101 = LINE ( 'NONE', #22631, #16930 ) ;
#6102 = LINE ( 'NONE', #9982, #6481 ) ;
#6103 = FACE_OUTER_BOUND ( 'NONE', #22912, .T. ) ;
#6104 = CARTESIAN_POINT ( 'NONE',  ( -117.3074641843675749, 85.22886158240835641, 90.00000000000000000 ) ) ;
#6105 = AXIS2_PLACEMENT_3D ( 'NONE', #22951, #19095, #6423 ) ;
#6106 = CARTESIAN_POINT ( 'NONE',  ( -72.64999999999994884, -87.33333333333338544, 3.000000000000001332 ) ) ;
#6107 = AXIS2_PLACEMENT_3D ( 'NONE', #20104, #71, #18182 ) ;
#6108 = CARTESIAN_POINT ( 'NONE',  ( -2.000000000000007550, -3.464101615137749945, 0.000000000000000000 ) ) ;
#6109 = AXIS2_PLACEMENT_3D ( 'NONE', #8819, #14498, #5303 ) ;
#6110 = DIRECTION ( 'NONE',  ( 1.000000000000000000, 0.000000000000000000, 0.000000000000000000 ) ) ;
#6111 = AXIS2_PLACEMENT_3D ( 'NONE', #15559, #10352, #8537 ) ;
#6112 = ORIENTED_EDGE ( 'NONE', *, *, #3116, .F. ) ;
#6113 = CARTESIAN_POINT ( 'NONE',  ( -79.99999999999995737, -138.0000000000000284, 3.000000000000000000 ) ) ;
#6114 = DIRECTION ( 'NONE',  ( -0.9423651898111408132, -0.3345860861306287348, 6.982962677686266711E-15 ) ) ;
#6115 = ORIENTED_EDGE ( 'NONE', *, *, #10546, .F. ) ;
#6116 = ORIENTED_EDGE ( 'NONE', *, *, #22745, .T. ) ;
#6117 = CYLINDRICAL_SURFACE ( 'NONE', #20378, 5.000000000000001776 ) ;
#6118 = CARTESIAN_POINT ( 'NONE',  ( 59.99999999999998579, -62.00000000000001421, 5.199999999999997513 ) ) ;
#6119 = LINE ( 'NONE', #22417, #7115 ) ;
#6120 = AXIS2_PLACEMENT_3D ( 'NONE', #12327, #15801, #17837 ) ;
#6121 = VERTEX_POINT ( 'NONE', #12098 ) ;
#6122 = AXIS2_PLACEMENT_3D ( 'NONE', #16494, #21919, #16740 ) ;
#6123 = CARTESIAN_POINT ( 'NONE',  ( 2.500000000000002220, 0.000000000000000000, 0.000000000000000000 ) ) ;
#6124 = LINE ( 'NONE', #6252, #2781 ) ;
#6125 = CIRCLE ( 'NONE', #8068, 20.30000000000000071 ) ;
#6126 = VECTOR ( 'NONE', #14760, 1000.000000000000000 ) ;
#6127 = CARTESIAN_POINT ( 'NONE',  ( 126.3653543294811499, 77.28387428943223370, 30.00000000000641620 ) ) ;
#6128 = ORIENTED_EDGE ( 'NONE', *, *, #1350, .T. ) ;
#6129 = CARTESIAN_POINT ( 'NONE',  ( 280.8700598572182798, 270.9755088701073191, 149.1320353020572611 ) ) ;
#6130 = DIRECTION ( 'NONE',  ( 1.000000000000000000, 0.000000000000000000, 0.000000000000000000 ) ) ;
#6131 = VECTOR ( 'NONE', #23378, 1000.000000000000114 ) ;
#6132 = CARTESIAN_POINT ( 'NONE',  ( 2.500000000000002220, -1.178949249685215417, 2.042000000000002036 ) ) ;
#6133 = VERTEX_POINT ( 'NONE', #20985 ) ;
#6134 = LINE ( 'NONE', #19036, #331 ) ;
#6135 = APPLICATION_CONTEXT ( 'automotive_design' ) ;
#6136 = EDGE_CURVE ( 'NONE', #19431, #18385, #2714, .T. ) ;
#6137 = DIRECTION ( 'NONE',  ( 0.000000000000000000, 2.618450529776319755E-15, 1.000000000000000000 ) ) ;
#6138 = DIRECTION ( 'NONE',  ( -1.000000000000000000, 6.640089860198304064E-16, 0.000000000000000000 ) ) ;
#6139 = DIRECTION ( 'NONE',  ( 0.000000000000000000, 2.618450529776313049E-15, 1.000000000000000000 ) ) ;
#6140 = EDGE_LOOP ( 'NONE', ( #2313, #6561, #10537, #21264 ) ) ;
#6141 = CIRCLE ( 'NONE', #5360, 4.057500000000000107 ) ;
#6142 = EDGE_LOOP ( 'NONE', ( #15647, #10259 ) ) ;
#6143 = AXIS2_PLACEMENT_3D ( 'NONE', #17929, #17680, #4661 ) ;
#6144 = CARTESIAN_POINT ( 'NONE',  ( 22.47082401081931735, -11.07878015919984804, 145.0000119999999697 ) ) ;
#6145 = AXIS2_PLACEMENT_3D ( 'NONE', #669, #14306, #21642 ) ;
#6146 = DIRECTION ( 'NONE',  ( -1.000000000000000000, 0.000000000000000000, 0.000000000000000000 ) ) ;
#6147 = VECTOR ( 'NONE', #21202, 1000.000000000000000 ) ;
#6148 = AXIS2_PLACEMENT_3D ( 'NONE', #6127, #23139, #2743 ) ;
#6149 = VERTEX_POINT ( 'NONE', #2622 ) ;
#6150 = DIRECTION ( 'NONE',  ( 0.000000000000000000, 2.618450529776326854E-15, 1.000000000000000000 ) ) ;
#6151 = CARTESIAN_POINT ( 'NONE',  ( -126.6510233831472050, 89.35617925171740694, 31.25900233431401531 ) ) ;
#6152 = ORIENTED_EDGE ( 'NONE', *, *, #18179, .F. ) ;
#6153 = CARTESIAN_POINT ( 'NONE',  ( 102.3500000000000227, -19.99999999999998934, 3.000000000000000000 ) ) ;
#6154 = EDGE_CURVE ( 'NONE', #2180, #19505, #14125, .T. ) ;
#6155 = ORIENTED_EDGE ( 'NONE', *, *, #2777, .T. ) ;
#6157 = AXIS2_PLACEMENT_3D ( 'NONE', #7354, #16527, #11123 ) ;
#6156 = AXIS2_PLACEMENT_3D ( 'NONE', #21759, #12514, #1354 ) ;
#6158 = MECHANICAL_DESIGN_GEOMETRIC_PRESENTATION_REPRESENTATION (  '', ( #6557 ), #5015 ) ;
#6160 = AXIS2_PLACEMENT_3D ( 'NONE', #21050, #15746, #8504 ) ;
#6159 = CARTESIAN_POINT ( 'NONE',  ( -90.00000000000000000, 3.053113317719180486E-13, 129.9038105676659711 ) ) ;
#6161 = ORIENTED_EDGE ( 'NONE', *, *, #11656, .F. ) ;
#6162 = ORIENTED_EDGE ( 'NONE', *, *, #3797, .F. ) ;
#6163 = FACE_OUTER_BOUND ( 'NONE', #12762, .T. ) ;
#6164 = CIRCLE ( 'NONE', #21602, 2.649999999999971934 ) ;
#6165 = VECTOR ( 'NONE', #10576, 1000.000000000000000 ) ;
#6166 = AXIS2_PLACEMENT_3D ( 'NONE', #22051, #8492, #5162 ) ;
#6167 = ADVANCED_FACE ( 'NONE', ( #4560 ), #4796, .F. ) ;
#6168 = PLANE ( 'NONE',  #16977 ) ;
#6169 = EDGE_CURVE ( 'NONE', #4516, #11736, #821, .T. ) ;
#6170 = FACE_OUTER_BOUND ( 'NONE', #22529, .T. ) ;
#6171 = CARTESIAN_POINT ( 'NONE',  ( 3.288228914120474133, -7.217643567644815406, -7.591235721156641247 ) ) ;
#6172 = CARTESIAN_POINT ( 'NONE',  ( 21.00000000000000355, 0.000000000000000000, 2.055000000000000160 ) ) ;
#6173 = ORIENTED_EDGE ( 'NONE', *, *, #23531, .T. ) ;
#6174 = LINE ( 'NONE', #13698, #5665 ) ;
#6175 = EDGE_CURVE ( 'NONE', #22916, #23140, #19512, .T. ) ;
#6176 = EDGE_LOOP ( 'NONE', ( #3477, #19113 ) ) ;
#6177 = PRODUCT_DEFINITION_FORMATION_WITH_SPECIFIED_SOURCE ( 'ANY', '', #20194, .NOT_KNOWN. ) ;
#6178 = CYLINDRICAL_SURFACE ( 'NONE', #4648, 2.500000000000002220 ) ;
#6179 = CARTESIAN_POINT ( 'NONE',  ( 5.000000000000000000, 4.685197434473814759, -5.637851296924623057E-15 ) ) ;
#6180 =( REPRESENTATION_RELATIONSHIP ('NONE','NONE', #10127, #11474 ) REPRESENTATION_RELATIONSHIP_WITH_TRANSFORMATION ( #3995 )SHAPE_REPRESENTATION_RELATIONSHIP( ) );
#6181 =( GEOMETRIC_REPRESENTATION_CONTEXT ( 3 ) GLOBAL_UNCERTAINTY_ASSIGNED_CONTEXT ( ( #18338 ) ) GLOBAL_UNIT_ASSIGNED_CONTEXT ( ( #959, #23186, #12017 ) ) REPRESENTATION_CONTEXT ( 'NONE', 'WORKASPACE' ) );
#6182 = AXIS2_PLACEMENT_3D ( 'NONE', #19789, #3239, #10651 ) ;
#6183 = VECTOR ( 'NONE', #5870, 1000.000000000000000 ) ;
#6184 = ORIENTED_EDGE ( 'NONE', *, *, #2841, .T. ) ;
#6185 = CARTESIAN_POINT ( 'NONE',  ( 10.40000000000000036, 0.000000000000000000, 5.000000000000001776 ) ) ;
#6186 = EDGE_LOOP ( 'NONE', ( #5177, #18357, #16047, #19165 ) ) ;
#6187 = CARTESIAN_POINT ( 'NONE',  ( -52.99999999999996447, -65.27838379715711881, 65.27838379715736039 ) ) ;
#6188 = CYLINDRICAL_SURFACE ( 'NONE', #16495, 160.0000000000000000 ) ;
#6189 = EDGE_LOOP ( 'NONE', ( #10646, #18661, #8224, #5375 ) ) ;
#6190 = CYLINDRICAL_SURFACE ( 'NONE', #14662, 2.649999999999971934 ) ;
#6191 = PRESENTATION_STYLE_ASSIGNMENT (( #3994 ) ) ;
#6192 = ORIENTED_EDGE ( 'NONE', *, *, #13021, .T. ) ;
#6193 = ADVANCED_FACE ( 'NONE', ( #3102 ), #10374, .F. ) ;
#6194 = CARTESIAN_POINT ( 'NONE',  ( 119.9257125005557043, -1087.686723660050802, -27.49999999999356248 ) ) ;
#6195 = CIRCLE ( 'NONE', #15817, 2.500000000000000444 ) ;
#6196 = EDGE_CURVE ( 'NONE', #15218, #3666, #4264, .T. ) ;
#6197 = CARTESIAN_POINT ( 'NONE',  ( 8.050035157498395932, -976.2746820519779476, -145.0000000000001421 ) ) ;
#6198 = CARTESIAN_POINT ( 'NONE',  ( 7.500000000000000000, 4.330127018922190096, -7.422398894150032511 ) ) ;
#6199 = CARTESIAN_POINT ( 'NONE',  ( -44.99999999999997868, -52.79999999999938609, 140.0000000000001421 ) ) ;
#6200 = ORIENTED_EDGE ( 'NONE', *, *, #16137, .F. ) ;
#6201 = CARTESIAN_POINT ( 'NONE',  ( -281.9771302778489712, 268.7755403010746704, 146.0571734979477014 ) ) ;
#6202 = EDGE_CURVE ( 'NONE', #13850, #3770, #22758, .T. ) ;
#6203 = PRODUCT_DEFINITION_SHAPE ( 'NONE', 'NONE',  #23827 ) ;
#6204 = ADVANCED_FACE ( 'NONE', ( #8553 ), #8308, .F. ) ;
#6206 = VERTEX_POINT ( 'NONE', #4685 ) ;
#6205 = ORIENTED_EDGE ( 'NONE', *, *, #14981, .F. ) ;
#6207 = DIRECTION ( 'NONE',  ( 1.000000000000000000, -1.408839003528726857E-14, -6.982962677686266711E-15 ) ) ;
#6208 = CARTESIAN_POINT ( 'NONE',  ( -7.500000000000000888, -4.330127018922198090, -7.564335161054497547 ) ) ;
#6209 = CYLINDRICAL_SURFACE ( 'NONE', #417, 7.500000000000007105 ) ;
#6210 = EDGE_CURVE ( 'NONE', #67, #10559, #1926, .T. ) ;
#6211 = CARTESIAN_POINT ( 'NONE',  ( 283.1956429438695295, 271.9582675804705332, 145.6220388411722979 ) ) ;
#6212 = CARTESIAN_POINT ( 'NONE',  ( -284.1822575857425477, 271.0140793454687582, -145.8708543776411375 ) ) ;
#6213 = PRODUCT_DEFINITION ( 'UNKNOWN', '', #5403, #9310 ) ;
#6214 = EDGE_LOOP ( 'NONE', ( #18718, #3810 ) ) ;
#6215 = EDGE_CURVE ( 'NONE', #13931, #3378, #5034, .T. ) ;
#6216 = DIRECTION ( 'NONE',  ( 0.000000000000000000, 0.000000000000000000, 1.000000000000000000 ) ) ;
#6217 = PLANE ( 'NONE',  #10619 ) ;
#6218 = CARTESIAN_POINT ( 'NONE',  ( 123.7141469857653391, -1093.380023028671530, 27.82653936295259811 ) ) ;
#6219 = ITEM_DEFINED_TRANSFORMATION ( 'NONE', 'NONE', #8880,  #11210 ) ;
#6220 = ORIENTED_EDGE ( 'NONE', *, *, #21929, .T. ) ;
#6221 = PLANE ( 'NONE',  #16339 ) ;
#6222 = ORIENTED_EDGE ( 'NONE', *, *, #16485, .T. ) ;
#6223 = FACE_OUTER_BOUND ( 'NONE', #2446, .T. ) ;
#6224 = LINE ( 'NONE', #20694, #5238 ) ;
#6225 = ORIENTED_EDGE ( 'NONE', *, *, #10037, .F. ) ;
#6226 = CARTESIAN_POINT ( 'NONE',  ( 8.050035159177506117, 23.72531794756937984, -145.0000000000000000 ) ) ;
#6227 = ORIENTED_EDGE ( 'NONE', *, *, #20849, .T. ) ;
#6228 = LINE ( 'NONE', #4031, #21163 ) ;
#6229 = DIRECTION ( 'NONE',  ( 0.000000000000000000, 0.000000000000000000, -1.000000000000000000 ) ) ;
#6230 = CARTESIAN_POINT ( 'NONE',  ( 0.000000000000000000, 0.000000000000000000, -90.00000000000000000 ) ) ;
#6231 = CARTESIAN_POINT ( 'NONE',  ( 20.00000000000000000, -1000.000000000000000, -150.0000000000000000 ) ) ;
#6232 = ADVANCED_FACE ( 'NONE', ( #19392 ), #11851, .F. ) ;
#6233 = CARTESIAN_POINT ( 'NONE',  ( -137.9031948627971076, -44.80746418436799416, 90.00000000000000000 ) ) ;
#6234 = DIRECTION ( 'NONE',  ( 0.000000000000000000, -1.000000000000000000, 0.000000000000000000 ) ) ;
#6235 = FACE_OUTER_BOUND ( 'NONE', #2768, .T. ) ;
#6236 = SHAPE_REPRESENTATION ( 'socket head cap screw_iso_ISO 4762 M5 x 16 - 16N', ( #11210 ), #9660 ) ;
#6237 = EDGE_LOOP ( 'NONE', ( #252, #9652, #93, #18602 ) ) ;
#6238 =( NAMED_UNIT ( * ) PLANE_ANGLE_UNIT ( ) SI_UNIT ( $, .RADIAN. ) );
#6239 = EDGE_CURVE ( 'NONE', #13321, #10209, #20395, .T. ) ;
#6240 = CARTESIAN_POINT ( 'NONE',  ( 9.999999999999998224, 1.224646799147352862E-15, 150.0000000000000284 ) ) ;
#6241 = LINE ( 'NONE', #205, #5018 ) ;
#6242 = ORIENTED_EDGE ( 'NONE', *, *, #4428, .F. ) ;
#6243 = EDGE_LOOP ( 'NONE', ( #15872, #22651, #4128, #4279 ) ) ;
#6244 = CARTESIAN_POINT ( 'NONE',  ( -35.00000000000000711, 4.286263797015737285E-15, -100.0000000000000000 ) ) ;
#6245 = DIRECTION ( 'NONE',  ( 0.000000000000000000, 0.000000000000000000, -1.000000000000000000 ) ) ;
#6246 = EDGE_CURVE ( 'NONE', #12980, #16635, #16449, .T. ) ;
#6247 = EDGE_CURVE ( 'NONE', #12957, #1216, #10734, .T. ) ;
#6248 = EDGE_CURVE ( 'NONE', #45, #493, #1405, .T. ) ;
#6249 = LINE ( 'NONE', #14109, #9838 ) ;
#6250 = ORIENTED_EDGE ( 'NONE', *, *, #21144, .F. ) ;
#6251 = CARTESIAN_POINT ( 'NONE',  ( 0.000000000000000000, 0.000000000000000000, 90.00000000000000000 ) ) ;
#6252 = CARTESIAN_POINT ( 'NONE',  ( -282.2000000000001023, 267.7999999999999545, -146.4928932188134354 ) ) ;
#6253 = CARTESIAN_POINT ( 'NONE',  ( -4.000000000000000000, 2.309401076758498483, -0.4999999999999927280 ) ) ;
#6254 = VERTEX_POINT ( 'NONE', #10975 ) ;
#6255 = CARTESIAN_POINT ( 'NONE',  ( 280.3118087683465660, 272.7329465209280670, 146.6795879751483369 ) ) ;
#6256 = CARTESIAN_POINT ( 'NONE',  ( 0.000000000000000000, 0.000000000000000000, 0.000000000000000000 ) ) ;
#6257 = CARTESIAN_POINT ( 'NONE',  ( 70.00000000000000000, -112.6666666666666714, 3.000000000000001332 ) ) ;
#6258 = VERTEX_POINT ( 'NONE', #18077 ) ;
#6259 = CARTESIAN_POINT ( 'NONE',  ( 281.7592670532758916, 269.1520027839447948, -145.8708543776411091 ) ) ;
#6260 = CONTEXT_DEPENDENT_SHAPE_REPRESENTATION ( #17751, #16163 ) ;
#6261 = CARTESIAN_POINT ( 'NONE',  ( 126.7787238282394924, 77.44864885511604768, 30.00000000000641975 ) ) ;
#6262 = DIRECTION ( 'NONE',  ( -1.000000000000000000, -0.000000000000000000, -0.000000000000000000 ) ) ;
#6263 = DIRECTION ( 'NONE',  ( -0.000000000000000000, -0.000000000000000000, 1.000000000000000000 ) ) ;
#6264 = AXIS2_PLACEMENT_3D ( 'NONE', #17505, #23294, #21262 ) ;
#6265 = EDGE_LOOP ( 'NONE', ( #8209, #7833 ) ) ;
#6266 = ORIENTED_EDGE ( 'NONE', *, *, #8229, .T. ) ;
#6267 = CARTESIAN_POINT ( 'NONE',  ( 124.4701338314433485, -1092.369831568443260, -27.49999999999351985 ) ) ;
#6268 = FACE_OUTER_BOUND ( 'NONE', #14302, .T. ) ;
#6269 = EDGE_CURVE ( 'NONE', #6379, #11094, #16152, .T. ) ;
#6270 = ADVANCED_FACE ( 'NONE', ( #14706, #14576, #22043, #23386 ), #16036, .T. ) ;
#6271 = ORIENTED_EDGE ( 'NONE', *, *, #19425, .T. ) ;
#6272 = CARTESIAN_POINT ( 'NONE',  ( 126.3653543294811499, 77.28387428943223370, 32.05500000000640171 ) ) ;
#6273 = ADVANCED_FACE ( 'NONE', ( #14246 ), #1531, .F. ) ;
#6274 = CARTESIAN_POINT ( 'NONE',  ( -126.8176664439037182, 89.11954614941086561, 31.65640384616917657 ) ) ;
#6275 = ORIENTED_EDGE ( 'NONE', *, *, #1611, .F. ) ;
#6276 = CARTESIAN_POINT ( 'NONE',  ( 25.00000000000004263, -37.41657386773938754, 169.9999999999999716 ) ) ;
#6277 = CIRCLE ( 'NONE', #14785, 5.249999999999949374 ) ;
#6278 = ORIENTED_EDGE ( 'NONE', *, *, #9712, .F. ) ;
#6279 = LINE ( 'NONE', #14148, #14868 ) ;
#6280 = CARTESIAN_POINT ( 'NONE',  ( 0.2500000000000002220, 0.000000000000000000, 0.000000000000000000 ) ) ;
#6281 = ORIENTED_EDGE ( 'NONE', *, *, #16521, .T. ) ;
#6282 = EDGE_LOOP ( 'NONE', ( #17146, #18799 ) ) ;
#6283 = CARTESIAN_POINT ( 'NONE',  ( -0.02511973781850462134, 4.877415612947412882, -3.751298745799839462 ) ) ;
#6284 = CARTESIAN_POINT ( 'NONE',  ( 0.000000000000000000, 1.865214261513747767E-15, -138.9999999999999716 ) ) ;
#6285 = DIRECTION ( 'NONE',  ( 0.000000000000000000, -2.618450529776313049E-15, -1.000000000000000000 ) ) ;
#6286 = LINE ( 'NONE', #17407, #15426 ) ;
#6287 = ORIENTED_EDGE ( 'NONE', *, *, #6495, .F. ) ;
#6288 = CARTESIAN_POINT ( 'NONE',  ( -45.00000000000000000, 269.9999999999999432, 0.000000000000000000 ) ) ;
#6289 = VECTOR ( 'NONE', #12571, 1000.000000000000000 ) ;
#6290 = ORIENTED_EDGE ( 'NONE', *, *, #21599, .F. ) ;
#6291 = CARTESIAN_POINT ( 'NONE',  ( 93.00000000000000000, -74.99999999999998579, 3.000000000000002665 ) ) ;
#6292 = ORIENTED_EDGE ( 'NONE', *, *, #2002, .T. ) ;
#6293 = ADVANCED_FACE ( 'NONE', ( #8921 ), #21570, .T. ) ;
#6294 = CARTESIAN_POINT ( 'NONE',  ( -18.83879023463320124, -16.51661848982829284, -145.0000000000000000 ) ) ;
#6295 = VERTEX_POINT ( 'NONE', #20223 ) ;
#6296 = CARTESIAN_POINT ( 'NONE',  ( 7.500000000000000888, 3.608439182435154269, -7.298562697733103732 ) ) ;
#6297 = DIRECTION ( 'NONE',  ( 0.000000000000000000, 0.000000000000000000, -1.000000000000000000 ) ) ;
#6298 = ORIENTED_EDGE ( 'NONE', *, *, #7394, .T. ) ;
#6299 = VECTOR ( 'NONE', #21540, 1000.000000000000000 ) ;
#6300 = CARTESIAN_POINT ( 'NONE',  ( -281.4928932188135491, 267.7999999999999545, 150.1999999999999886 ) ) ;
#6301 = ORIENTED_EDGE ( 'NONE', *, *, #10889, .F. ) ;
#6302 = AXIS2_PLACEMENT_3D ( 'NONE', #9333, #14764, #14882 ) ;
#6303 = UNCERTAINTY_MEASURE_WITH_UNIT (LENGTH_MEASURE( 1.000000000000000082E-05 ), #13864, 'distance_accuracy_value', 'NONE');
#6304 = CARTESIAN_POINT ( 'NONE',  ( 3.000000000000002220, 2.486033002269127373E-15, 20.30000000000000071 ) ) ;
#6305 = DIRECTION ( 'NONE',  ( 0.000000000000000000, 0.000000000000000000, 1.000000000000000000 ) ) ;
#6306 = CARTESIAN_POINT ( 'NONE',  ( 155.0000000000000284, -210.0000000000003411, -27.49999999999350209 ) ) ;
#6307 = DIRECTION ( 'NONE',  ( 0.000000000000000000, 2.618450529776326854E-15, 1.000000000000000000 ) ) ;
#6308 = EDGE_LOOP ( 'NONE', ( #2280, #5317, #23050, #10213 ) ) ;
#6309 = LINE ( 'NONE', #2695, #3424 ) ;
#6310 = CIRCLE ( 'NONE', #19809, 20.00000000000000000 ) ;
#6312 = VERTEX_POINT ( 'NONE', #5052 ) ;
#6311 = ORIENTED_EDGE ( 'NONE', *, *, #3400, .F. ) ;
#6313 = AXIS2_PLACEMENT_3D ( 'NONE', #6104, #12073, #13526 ) ;
#6314 = CARTESIAN_POINT ( 'NONE',  ( -163.0000000000005400, -494.4690652294798383, -29.99999999999344880 ) ) ;
#6315 = CARTESIAN_POINT ( 'NONE',  ( -2.500000000000000000, 7.216878364870324525, -7.063244554130001518 ) ) ;
#6316 = CARTESIAN_POINT ( 'NONE',  ( -34.75000000000005684, 100.0000000000000000, 150.2000000000009550 ) ) ;
#6317 = DIRECTION ( 'NONE',  ( 0.000000000000000000, 0.000000000000000000, 1.000000000000000000 ) ) ;
#6318 = EDGE_CURVE ( 'NONE', #9451, #20774, #7692, .T. ) ;
#6319 = CARTESIAN_POINT ( 'NONE',  ( 80.00000000000001421, -56.79999999999913030, 250.0000000000000000 ) ) ;
#6320 = EDGE_LOOP ( 'NONE', ( #12613, #14724, #19571, #19035 ) ) ;
#6321 = ADVANCED_FACE ( 'NONE', ( #5153 ), #10810, .F. ) ;
#6322 = CARTESIAN_POINT ( 'NONE',  ( -9.999999999999998224, 0.000000000000000000, 200.0000119999999981 ) ) ;
#6323 = DIRECTION ( 'NONE',  ( -1.000000000000000000, -0.000000000000000000, -0.000000000000000000 ) ) ;
#6324 = DIRECTION ( 'NONE',  ( -0.000000000000000000, -0.000000000000000000, 1.000000000000000000 ) ) ;
#6325 = EDGE_CURVE ( 'NONE', #16985, #2548, #10868, .T. ) ;
#6326 = EDGE_CURVE ( 'NONE', #14669, #17715, #7079, .T. ) ;
#6327 = CONTEXT_DEPENDENT_SHAPE_REPRESENTATION ( #13430, #609 ) ;
#6328 = ORIENTED_EDGE ( 'NONE', *, *, #10525, .F. ) ;
#6330 = FACE_OUTER_BOUND ( 'NONE', #12863, .T. ) ;
#6329=STYLED_ITEM('',(#23927),#12057);
#6331 = EDGE_LOOP ( 'NONE', ( #16612, #175, #18420, #11661 ) ) ;
#6332 = CARTESIAN_POINT ( 'NONE',  ( -285.2000000000014666, -132.2000000000000455, -146.4928932188134070 ) ) ;
#6333 = AXIS2_PLACEMENT_3D ( 'NONE', #23472, #10839, #14339 ) ;
#6334 = DIRECTION ( 'NONE',  ( 0.000000000000000000, 0.000000000000000000, -1.000000000000000000 ) ) ;
#6335 = VERTEX_POINT ( 'NONE', #3206 ) ;
#6336 = CARTESIAN_POINT ( 'NONE',  ( 22.46856765566318614, 11.08409875790209753, -145.0000000000000000 ) ) ;
#6337 = ORIENTED_EDGE ( 'NONE', *, *, #2804, .F. ) ;
#6338 = AXIS2_PLACEMENT_3D ( 'NONE', #18806, #11265, #2028 ) ;
#6339 = LINE ( 'NONE', #11939, #1064 ) ;
#6340 = EDGE_CURVE ( 'NONE', #9973, #10543, #3457, .T. ) ;
#6341 = FACE_OUTER_BOUND ( 'NONE', #21118, .T. ) ;
#6342 = CYLINDRICAL_SURFACE ( 'NONE', #20760, 145.0000000000000284 ) ;
#6343 = DIRECTION ( 'NONE',  ( 1.000000000000000000, 0.000000000000000000, 0.000000000000000000 ) ) ;
#6344 = FACE_BOUND ( 'NONE', #3412, .T. ) ;
#6345 = VERTEX_POINT ( 'NONE', #7187 ) ;
#6346 = AXIS2_PLACEMENT_3D ( 'NONE', #9368, #20456, #184 ) ;
#6347 = DIRECTION ( 'NONE',  ( -1.000000000000000000, -0.000000000000000000, -0.000000000000000000 ) ) ;
#6348 = DIRECTION ( 'NONE',  ( 0.000000000000000000, 0.000000000000000000, -1.000000000000000000 ) ) ;
#6349 = ORIENTED_EDGE ( 'NONE', *, *, #16677, .T. ) ;
#6350 = VERTEX_POINT ( 'NONE', #18193 ) ;
#6351 = DIRECTION ( 'NONE',  ( 0.000000000000000000, 0.000000000000000000, 1.000000000000000000 ) ) ;
#6353 = VECTOR ( 'NONE', #17209, 1000.000000000000000 ) ;
#6352 = PLANE ( 'NONE',  #17304 ) ;
#6354 = LINE ( 'NONE', #11957, #4826 ) ;
#6355 = VECTOR ( 'NONE', #7477, 1000.000000000000000 ) ;
#6356 = CIRCLE ( 'NONE', #21383, 2.500000000000002220 ) ;
#6357 = DIRECTION ( 'NONE',  ( 0.000000000000000000, 0.000000000000000000, -1.000000000000000000 ) ) ;
#6358 = CYLINDRICAL_SURFACE ( 'NONE', #16306, 145.0000000000000284 ) ;
#6359 = EDGE_CURVE ( 'NONE', #12563, #21417, #1640, .T. ) ;
#6360 = CARTESIAN_POINT ( 'NONE',  ( -10.12668159690567649, 1.256356190803088863E-15, -9.999999999999998224 ) ) ;
#6361 = EDGE_CURVE ( 'NONE', #18342, #880, #19248, .T. ) ;
#6362 = ORIENTED_EDGE ( 'NONE', *, *, #2318, .T. ) ;
#6363 = DIRECTION ( 'NONE',  ( 0.000000000000000000, 0.000000000000000000, -1.000000000000000000 ) ) ;
#6364 = CARTESIAN_POINT ( 'NONE',  ( 79.04925354955072692, 121.5574576620408322, -90.00000000000000000 ) ) ;
#6365 = EDGE_CURVE ( 'NONE', #2692, #14837, #9138, .T. ) ;
#6366 = ORIENTED_EDGE ( 'NONE', *, *, #16200, .T. ) ;
#6367 = CARTESIAN_POINT ( 'NONE',  ( 1.500000000000001332, 0.000000000000000000, 0.000000000000000000 ) ) ;
#6368 =( BOUNDED_SURFACE ( )  B_SPLINE_SURFACE ( 3, 2, ( 
 ( #9918, #17402, #12008 ),
 ( #22815, #22689, #4471 ),
 ( #11877, #379, #841 ),
 ( #15484, #19311, #19185 ),
 ( #2770, #20756, #7851 ),
 ( #22566, #4089, #6283 ) ),
 .UNSPECIFIED., .F., .F., .F. ) 
 B_SPLINE_SURFACE_WITH_KNOTS ( ( 4, 2, 4 ),
 ( 3, 3 ),
 ( 0.02032853247518126225, 0.02278863295364821212, 0.02524873343211516200 ),
 ( 0.000000000000000000, 1.000000000000000000 ),
 .UNSPECIFIED. ) 
 GEOMETRIC_REPRESENTATION_ITEM ( )  RATIONAL_B_SPLINE_SURFACE ( (
 ( 1.000000000000000000, 0.8047781615896835161, 1.000000000000000000),
 ( 1.000000000000000000, 0.8123767586291043008, 1.000000000000000000),
 ( 1.000000000000000000, 0.8190662415562011134, 1.000000000000000000),
 ( 1.000000000000000000, 0.8192361015671398849, 1.000000000000000000),
 ( 1.000000000000000000, 0.8126135807102121689, 1.000000000000000000),
 ( 1.000000000000000000, 0.8047712338318585568, 1.000000000000000000) ) ) 
 REPRESENTATION_ITEM ( '' )  SURFACE ( )  );
#6369 = EDGE_CURVE ( 'NONE', #874, #10912, #2266, .T. ) ;
#6371 = AXIS2_PLACEMENT_3D ( 'NONE', #3695, #20015, #11109 ) ;
#6370 = CONTEXT_DEPENDENT_SHAPE_REPRESENTATION ( #19090, #3016 ) ;
#6372 = PLANE ( 'NONE',  #20441 ) ;
#6373 = PRODUCT_RELATED_PRODUCT_CATEGORY ( 'part', '', ( #3218 ) ) ;
#6374 = EDGE_CURVE ( 'NONE', #2426, #11453, #82, .T. ) ;
#6375 = DIRECTION ( 'NONE',  ( 0.000000000000000000, -0.5000000000000011102, -0.8660254037844379305 ) ) ;
#6376 = DIRECTION ( 'NONE',  ( -1.000000000000000000, -0.000000000000000000, -0.000000000000000000 ) ) ;
#6377 = VECTOR ( 'NONE', #16983, 1000.000000000000000 ) ;
#6378 = ORIENTED_EDGE ( 'NONE', *, *, #8160, .F. ) ;
#6379 = VERTEX_POINT ( 'NONE', #2223 ) ;
#6380 = FACE_BOUND ( 'NONE', #12034, .T. ) ;
#6381 = CARTESIAN_POINT ( 'NONE',  ( 282.1999999999999886, 267.7999999999999545, 146.4928932188134922 ) ) ;
#6382 = ORIENTED_EDGE ( 'NONE', *, *, #5722, .F. ) ;
#6383 = AXIS2_PLACEMENT_3D ( 'NONE', #10030, #2628, #22803 ) ;
#6384 = ORIENTED_EDGE ( 'NONE', *, *, #21629, .F. ) ;
#6385 = CARTESIAN_POINT ( 'NONE',  ( 280.8708543776410806, 271.0140793454687582, 149.1822575857424624 ) ) ;
#6386 = FACE_OUTER_BOUND ( 'NONE', #8801, .T. ) ;
#6387 = ORIENTED_EDGE ( 'NONE', *, *, #12157, .F. ) ;
#6388 = DIRECTION ( 'NONE',  ( -0.000000000000000000, -0.000000000000000000, 1.000000000000000000 ) ) ;
#6389 = TOROIDAL_SURFACE ( 'NONE', #12611, 24.69999999999999929, 0.3000000000000007661 ) ;
#6390 = AXIS2_PLACEMENT_3D ( 'NONE', #19528, #12109, #11994 ) ;
#6391 = ORIENTED_EDGE ( 'NONE', *, *, #5599, .T. ) ;
#6392 = DIRECTION ( 'NONE',  ( 0.000000000000000000, 0.000000000000000000, -1.000000000000000000 ) ) ;
#6393 = CARTESIAN_POINT ( 'NONE',  ( 0.000000000000000000, 272.9999999999999432, 3.330669073875469621E-16 ) ) ;
#6394 = ORIENTED_EDGE ( 'NONE', *, *, #5129, .T. ) ;
#6395 = ORIENTED_EDGE ( 'NONE', *, *, #18076, .T. ) ;
#6396 = CARTESIAN_POINT ( 'NONE',  ( -64.99999999999995737, -52.79999999999965610, 65.00000000000017053 ) ) ;
#6397 = PRODUCT_DEFINITION_SHAPE ( 'NONE', 'NONE',  #23836 ) ;
#6398 = FACE_OUTER_BOUND ( 'NONE', #5072, .T. ) ;
#6399 = ADVANCED_FACE ( 'NONE', ( #6103 ), #20008, .T. ) ;
#6400 = EDGE_CURVE ( 'NONE', #21286, #22490, #9240, .T. ) ;
#6401 = CIRCLE ( 'NONE', #2532, 5.249999999999949374 ) ;
#6402 = ADVANCED_FACE ( 'NONE', ( #11331 ), #4297, .F. ) ;
#6403 = DIRECTION ( 'NONE',  ( 0.000000000000000000, 0.000000000000000000, 1.000000000000000000 ) ) ;
#6404 = DIRECTION ( 'NONE',  ( 1.000000000000000000, 0.000000000000000000, 0.000000000000000000 ) ) ;
#6405 = EDGE_LOOP ( 'NONE', ( #20168, #12479, #934, #4665, #13030 ) ) ;
#6406 = CARTESIAN_POINT ( 'NONE',  ( -5.147825380260782957, -5.688155668810408017, -7.450218641351304960 ) ) ;
#6407 = CIRCLE ( 'NONE', #16815, 2.499999999999998668 ) ;
#6408 = ORIENTED_EDGE ( 'NONE', *, *, #5482, .T. ) ;
#6409 = ADVANCED_BREP_SHAPE_REPRESENTATION ( '', ( #3850, #11210 ), #18837 ) ;
#6410 = ORIENTED_EDGE ( 'NONE', *, *, #15714, .F. ) ;
#6411 = CARTESIAN_POINT ( 'NONE',  ( -64.99999999999997158, -52.79999999999974847, 35.00000000000017764 ) ) ;
#6412 = ORIENTED_EDGE ( 'NONE', *, *, #16214, .F. ) ;
#6413 = AXIS2_PLACEMENT_3D ( 'NONE', #538, #7899, #429 ) ;
#6414 = DIRECTION ( 'NONE',  ( 0.000000000000000000, 0.000000000000000000, 1.000000000000000000 ) ) ;
#6415 = DIRECTION ( 'NONE',  ( 0.000000000000000000, 0.000000000000000000, 1.000000000000000000 ) ) ;
#6416 = ORIENTED_EDGE ( 'NONE', *, *, #14942, .T. ) ;
#6417 = AXIS2_PLACEMENT_3D ( 'NONE', #18748, #13148, #3782 ) ;
#6418 = CARTESIAN_POINT ( 'NONE',  ( -281.4928932188135491, 267.7999999999999545, 147.1999999999999886 ) ) ;
#6419 = CARTESIAN_POINT ( 'NONE',  ( 119.6158142514525622, -1087.367367941136990, -29.99999999999356604 ) ) ;
#6420 = EDGE_LOOP ( 'NONE', ( #20134, #11761, #17500, #10580 ) ) ;
#6421 = LINE ( 'NONE', #15864, #20809 ) ;
#6422 = CARTESIAN_POINT ( 'NONE',  ( 282.2000000000008981, 9.787860418609723716E-13, 0.000000000000000000 ) ) ;
#6423 = DIRECTION ( 'NONE',  ( -0.3090169943749517811, 0.9510565162951520879, 0.000000000000000000 ) ) ;
#6424 = CARTESIAN_POINT ( 'NONE',  ( -7.499999999999999112, 41.99999999999998579, -100.0000000000000000 ) ) ;
#6425 = EDGE_LOOP ( 'NONE', ( #6744, #9086, #7475, #10173, #12108 ) ) ;
#6426 = LINE ( 'NONE', #6556, #13133 ) ;
#6427 = AXIS2_PLACEMENT_3D ( 'NONE', #1598, #17908, #7392 ) ;
#6428 =( NAMED_UNIT ( * ) PLANE_ANGLE_UNIT ( ) SI_UNIT ( $, .RADIAN. ) );
#6430 = ORIENTED_EDGE ( 'NONE', *, *, #4132, .F. ) ;
#6429 = ORIENTED_EDGE ( 'NONE', *, *, #10475, .F. ) ;
#6431 = CARTESIAN_POINT ( 'NONE',  ( -145.2408737859499581, -1078.096661784571324, 30.00000000000653699 ) ) ;
#6432 = CARTESIAN_POINT ( 'NONE',  ( 7.897825807688775512, 1.532833846124499910, -7.633607627188418121 ) ) ;
#6433 = DIRECTION ( 'NONE',  ( -0.000000000000000000, 0.000000000000000000, -1.000000000000000000 ) ) ;
#6434 = CARTESIAN_POINT ( 'NONE',  ( -7.499999999999997335, 34.18698582794336005, -100.0000000000000000 ) ) ;
#6435 = CARTESIAN_POINT ( 'NONE',  ( 0.2500000000000002220, 0.000000000000000000, 0.000000000000000000 ) ) ;
#6436 = DIRECTION ( 'NONE',  ( -1.000000000000000000, 1.408839003528726857E-14, 6.982962677686266711E-15 ) ) ;
#6437 = ORIENTED_EDGE ( 'NONE', *, *, #19331, .T. ) ;
#6438 = VECTOR ( 'NONE', #3846, 1000.000000000000000 ) ;
#6439 = B_SPLINE_CURVE_WITH_KNOTS ( 'NONE', 3,
 ( #15705, #3128, #19307, #13686, #21005, #4466 ),
 .UNSPECIFIED., .F., .F.,
 ( 4, 2, 4 ),
 ( -3.640115492409406142E-06, 0.0002066546034006526487, 0.0004169493222937146744 ),
 .UNSPECIFIED. ) ;
#6440 = DIRECTION ( 'NONE',  ( -0.9510565162951557516, 0.3090169943749406234, 0.000000000000000000 ) ) ;
#6441 = CIRCLE ( 'NONE', #21862, 2.041999999999999815 ) ;
#6442 = LINE ( 'NONE', #775, #14262 ) ;
#6443 = CARTESIAN_POINT ( 'NONE',  ( 279.9999999999999432, 272.9999999999999432, -144.9999999999999716 ) ) ;
#6444 = CONTEXT_DEPENDENT_SHAPE_REPRESENTATION ( #1807, #21043 ) ;
#6445 = EDGE_CURVE ( 'NONE', #10663, #11416, #18841, .T. ) ;
#6446 = ORIENTED_EDGE ( 'NONE', *, *, #2101, .F. ) ;
#6447 = DIRECTION ( 'NONE',  ( 1.000000000000000000, -0.000000000000000000, -0.000000000000000000 ) ) ;
#6448 = ORIENTED_EDGE ( 'NONE', *, *, #4596, .F. ) ;
#6449 = DIRECTION ( 'NONE',  ( -1.000000000000000000, -0.000000000000000000, -0.000000000000000000 ) ) ;
#6450 = CARTESIAN_POINT ( 'NONE',  ( 0.000000000000000000, -2.357898499370431722, 2.818925648462311528E-15 ) ) ;
#6451 = VERTEX_POINT ( 'NONE', #11223 ) ;
#6452 = FACE_OUTER_BOUND ( 'NONE', #10949, .T. ) ;
#6453 = ORIENTED_EDGE ( 'NONE', *, *, #8341, .T. ) ;
#6454 = FACE_OUTER_BOUND ( 'NONE', #5735, .T. ) ;
#6455 = CARTESIAN_POINT ( 'NONE',  ( -79.04925354955163641, -121.5574576620402496, 90.00000000000000000 ) ) ;
#6456 = EDGE_CURVE ( 'NONE', #6907, #23173, #740, .T. ) ;
#6457 = CARTESIAN_POINT ( 'NONE',  ( 24.33333333333333215, -89.99999999999998579, 3.000000000000001332 ) ) ;
#6458 = DIRECTION ( 'NONE',  ( 0.000000000000000000, 0.000000000000000000, -1.000000000000000000 ) ) ;
#6459 = DIRECTION ( 'NONE',  ( -5.618537574013950123E-17, -3.483493295888648978E-15, -1.000000000000000000 ) ) ;
#6460 = EDGE_CURVE ( 'NONE', #8431, #19800, #4989, .T. ) ;
#6461 = DIRECTION ( 'NONE',  ( 1.000000000000000000, 0.000000000000000000, 0.000000000000000000 ) ) ;
#6462 = ORIENTED_EDGE ( 'NONE', *, *, #26, .F. ) ;
#6463 = CARTESIAN_POINT ( 'NONE',  ( -285.2000000000006708, 90.00000000000100897, 37.64999999999996305 ) ) ;
#6464 = VECTOR ( 'NONE', #2574, 1000.000000000000000 ) ;
#6465 = LINE ( 'NONE', #12305, #19674 ) ;
#6466 = EDGE_CURVE ( 'NONE', #7547, #16501, #22329, .T. ) ;
#6467 = ORIENTED_EDGE ( 'NONE', *, *, #16661, .F. ) ;
#6468 = EDGE_LOOP ( 'NONE', ( #6878, #11108, #20530, #2887 ) ) ;
#6469 = CIRCLE ( 'NONE', #13835, 2.649999999999985700 ) ;
#6470 = FACE_OUTER_BOUND ( 'NONE', #18190, .T. ) ;
#6471 = CARTESIAN_POINT ( 'NONE',  ( -146.4450000000001069, -494.4690652294807478, 27.50000000000642331 ) ) ;
#6472 = DIRECTION ( 'NONE',  ( 0.000000000000000000, -1.000000000000000000, 0.000000000000000000 ) ) ;
#6473 = CARTESIAN_POINT ( 'NONE',  ( 131.5246926503482996, 82.01375679560405274, 30.33200430454443719 ) ) ;
#6474 = CARTESIAN_POINT ( 'NONE',  ( 100.0000000000000000, -1420.000000000000000, -145.0000000000001705 ) ) ;
#6475 = DIRECTION ( 'NONE',  ( 0.000000000000000000, 0.000000000000000000, 1.000000000000000000 ) ) ;
#6476 = VERTEX_POINT ( 'NONE', #18761 ) ;
#6477 = DIRECTION ( 'NONE',  ( 1.000000000000000000, 0.000000000000000000, 0.000000000000000000 ) ) ;
#6478 = DIRECTION ( 'NONE',  ( 1.000000000000000000, 0.000000000000000000, -0.000000000000000000 ) ) ;
#6479 = CIRCLE ( 'NONE', #17661, 145.0000000000000284 ) ;
#6480 = LINE ( 'NONE', #19387, #10603 ) ;
#6481 = VECTOR ( 'NONE', #15542, 1000.000000000000000 ) ;
#6482 = EDGE_LOOP ( 'NONE', ( #16799, #8301, #17710, #7417 ) ) ;
#6483 = DIRECTION ( 'NONE',  ( -0.000000000000000000, 1.000000000000000000, -3.469446951953613794E-15 ) ) ;
#6484 = AXIS2_PLACEMENT_3D ( 'NONE', #11956, #13999, #4779 ) ;
#6485 = DIRECTION ( 'NONE',  ( 0.9289202219288174023, 0.3702799228849933955, 6.982962677686265922E-15 ) ) ;
#6486 = FACE_OUTER_BOUND ( 'NONE', #622, .T. ) ;
#6487 = DIRECTION ( 'NONE',  ( -0.000000000000000000, -0.000000000000000000, -1.000000000000000000 ) ) ;
#6488 = CARTESIAN_POINT ( 'NONE',  ( -282.2000000000013529, -89.99999999999897682, 26.98333333333330231 ) ) ;
#6489 = ORIENTED_EDGE ( 'NONE', *, *, #15338, .T. ) ;
#6490 = VERTEX_POINT ( 'NONE', #15302 ) ;
#6491 = DIRECTION ( 'NONE',  ( 0.000000000000000000, 0.000000000000000000, 1.000000000000000000 ) ) ;
#6492 = CARTESIAN_POINT ( 'NONE',  ( 281.4928932188133217, 267.7999999999999545, 147.1999999999999886 ) ) ;
#6493 = EDGE_CURVE ( 'NONE', #18246, #6451, #22633, .T. ) ;
#6494 = ORIENTED_EDGE ( 'NONE', *, *, #12476, .F. ) ;
#6495 = EDGE_CURVE ( 'NONE', #18184, #15856, #16989, .T. ) ;
#6496 = PRODUCT ( 'hex flange nut gradea_iso_ISO - 4161 - M10 - N', 'hex flange nut gradea_iso_ISO - 4161 - M10 - N', '', ( #2135 ) ) ;
#6497 = VECTOR ( 'NONE', #22041, 1000.000000000000114 ) ;
#6498 = VECTOR ( 'NONE', #2227, 1000.000000000000000 ) ;
#6499 = ORIENTED_EDGE ( 'NONE', *, *, #1639, .T. ) ;
#6500 = DIRECTION ( 'NONE',  ( -1.000000000000000000, 1.408839003528726857E-14, 6.982962677686266711E-15 ) ) ;
#6501 = CIRCLE ( 'NONE', #16174, 5.249999999999949374 ) ;
#6502 = EDGE_CURVE ( 'NONE', #4339, #9995, #197, .T. ) ;
#6503 = CARTESIAN_POINT ( 'NONE',  ( -126.7571989378452599, 89.20549877611294676, 31.53022738271492997 ) ) ;
#6504 = VERTEX_POINT ( 'NONE', #13271 ) ;
#6505 = CARTESIAN_POINT ( 'NONE',  ( -134.5566256099407099, -1076.938388239962933, -29.66799569545555215 ) ) ;
#6506 = EDGE_CURVE ( 'NONE', #218, #2340, #3040, .T. ) ;
#6507 = AXIS2_PLACEMENT_3D ( 'NONE', #5781, #6130, #2499 ) ;
#6508 = SHAPE_REPRESENTATION ( 'socket head cap screw_iso_ISO 4762 M5 x 25 - 25N', ( #11210 ), #16951 ) ;
#6509 = ORIENTED_EDGE ( 'NONE', *, *, #7837, .T. ) ;
#6510 = CARTESIAN_POINT ( 'NONE',  ( -59.99999999999996447, -59.79999999999998295, 5.199999999999991296 ) ) ;
#6511 = CARTESIAN_POINT ( 'NONE',  ( 91.18044947428791147, 112.7436279071541776, -2.775557561562891351E-14 ) ) ;
#6512 = ORIENTED_EDGE ( 'NONE', *, *, #2900, .F. ) ;
#6513 = ORIENTED_EDGE ( 'NONE', *, *, #22859, .F. ) ;
#6514 = CARTESIAN_POINT ( 'NONE',  ( 133.2563391751591837, 79.16925799295223953, -27.62591505085368127 ) ) ;
#6515 = AXIS2_PLACEMENT_3D ( 'NONE', #4406, #5979, #11329 ) ;
#6516 = CARTESIAN_POINT ( 'NONE',  ( 0.000000000000000000, -132.2000000000000455, -7.703011046602857601E-15 ) ) ;
#6517 = AXIS2_PLACEMENT_3D ( 'NONE', #19965, #5597, #3425 ) ;
#6518 = VECTOR ( 'NONE', #2107, 1000.000000000000000 ) ;
#6520 = CARTESIAN_POINT ( 'NONE',  ( -146.0000000000000853, -204.4690652294807478, 30.00000000000641620 ) ) ;
#6519 = AXIS2_PLACEMENT_3D ( 'NONE', #14469, #19515, #3210 ) ;
#6521 = DIRECTION ( 'NONE',  ( -0.000000000000000000, -0.000000000000000000, 1.000000000000000000 ) ) ;
#6522 = AXIS2_PLACEMENT_3D ( 'NONE', #5832, #22722, #15021 ) ;
#6523 = VECTOR ( 'NONE', #21222, 1000.000000000000114 ) ;
#6524 = ORIENTED_EDGE ( 'NONE', *, *, #13507, .T. ) ;
#6525 = ADVANCED_FACE ( 'NONE', ( #7551 ), #22513, .T. ) ;
#6526 = DIRECTION ( 'NONE',  ( 0.000000000000000000, 1.000000000000000000, -3.469446951953614189E-15 ) ) ;
#6527 =( NAMED_UNIT ( * ) SI_UNIT ( $, .STERADIAN. ) SOLID_ANGLE_UNIT ( ) );
#6528 = B_SPLINE_CURVE_WITH_KNOTS ( 'NONE', 3,
 ( #4838, #15498, #22827, #22938, #965, #21140, #2886, #22711, #6294, #23059, #3011, #23191, #13595, #4362, #21024, #13951, #11769, #10289, #21269, #4484, #19321, #2669, #1088, #17413, #853, #10168, #19429, #15610, #17630, #2783, #10544, #17880, #23558, #12497 ),
 .UNSPECIFIED., .F., .F.,
 ( 4, 2, 2, 2, 2, 2, 2, 2, 2, 2, 2, 2, 2, 2, 2, 2, 4 ),
 ( 0.7500000000000000000, 0.7812500000000000000, 0.8125000000000000000, 0.8437500000000000000, 0.8750000000000000000, 0.9062500000000000000, 0.9375000000000000000, 0.9687500000000000000, 1.000000000000000000, 1.031250000000000000, 1.062500000000000000, 1.093750000000000000, 1.125000000000000000, 1.156250000000000000, 1.187500000000000000, 1.218750000000000000, 1.250000000000000000 ),
 .UNSPECIFIED. ) ;
#6529 = VERTEX_POINT ( 'NONE', #9379 ) ;
#6530 = ORIENTED_EDGE ( 'NONE', *, *, #16274, .F. ) ;
#6531 = VECTOR ( 'NONE', #6067, 1000.000000000000000 ) ;
#6532 = DIRECTION ( 'NONE',  ( 0.000000000000000000, -3.495664435217746987E-15, 1.000000000000000000 ) ) ;
#6533 = EDGE_CURVE ( 'NONE', #14975, #4130, #18469, .T. ) ;
#6535 = VECTOR ( 'NONE', #7741, 1000.000000000000000 ) ;
#6534 = STYLED_ITEM ( 'NONE', ( #5307 ), #16222 ) ;
#6536 = EDGE_LOOP ( 'NONE', ( #10791, #14486, #23778, #16397 ) ) ;
#6537 = AXIS2_PLACEMENT_3D ( 'NONE', #20951, #19818, #8602 ) ;
#6539 = ADVANCED_FACE ( 'NONE', ( #20335 ), #3798, .F. ) ;
#6538 = CARTESIAN_POINT ( 'NONE',  ( -7.497491405671719455, -144.8060344827586334, 90.00000000000000000 ) ) ;
#6540 = AXIS2_PLACEMENT_3D ( 'NONE', #20554, #22125, #18384 ) ;
#6541 = CIRCLE ( 'NONE', #5385, 2.500000000000002220 ) ;
#6542 = B_SPLINE_CURVE_WITH_KNOTS ( 'NONE', 3,
 ( #5816, #30, #3736, #9202, #8966, #11154 ),
 .UNSPECIFIED., .F., .F.,
 ( 4, 2, 4 ),
 ( 0.004444412883774334112, 0.006655097293744431999, 0.008865781703714530754 ),
 .UNSPECIFIED. ) ;
#6543 = FACE_OUTER_BOUND ( 'NONE', #13817, .T. ) ;
#6544 = AXIS2_PLACEMENT_3D ( 'NONE', #20106, #5383, #7307 ) ;
#6545 = AXIS2_PLACEMENT_3D ( 'NONE', #16289, #23631, #7087 ) ;
#6546 = ORIENTED_EDGE ( 'NONE', *, *, #7064, .T. ) ;
#6547 = CARTESIAN_POINT ( 'NONE',  ( -280.0000000000000568, 272.9999999999999432, 145.0000000000000284 ) ) ;
#6548 = ORIENTED_EDGE ( 'NONE', *, *, #21176, .F. ) ;
#6549 = CARTESIAN_POINT ( 'NONE',  ( -5.000000000000001776, 0.000000000000000000, -9.974600000000000577 ) ) ;
#6550 =( NAMED_UNIT ( * ) PLANE_ANGLE_UNIT ( ) SI_UNIT ( $, .RADIAN. ) );
#6551 = DIRECTION ( 'NONE',  ( 1.000000000000000000, 0.000000000000000000, 0.000000000000000000 ) ) ;
#6552 = DIRECTION ( 'NONE',  ( -0.000000000000000000, 1.000000000000000000, -3.469446951953613794E-15 ) ) ;
#6553 = VERTEX_POINT ( 'NONE', #22273 ) ;
#6555 = AXIS2_PLACEMENT_3D ( 'NONE', #23761, #20495, #22068 ) ;
#6554 = STYLED_ITEM ( 'NONE', ( #16607 ), #15670 ) ;
#6556 = CARTESIAN_POINT ( 'NONE',  ( 2.500000000000000000, -1.178949249685218081, -2.041999999999998039 ) ) ;
#6557 = STYLED_ITEM ( 'NONE', ( #19569 ), #3229 ) ;
#6558 = AXIS2_PLACEMENT_3D ( 'NONE', #4133, #9477, #18871 ) ;
#6559 = AXIS2_PLACEMENT_3D ( 'NONE', #6664, #12393, #23315 ) ;
#6560 = CIRCLE ( 'NONE', #10449, 7.500000000000000888 ) ;
#6562 = VERTEX_POINT ( 'NONE', #3918 ) ;
#6561 = ORIENTED_EDGE ( 'NONE', *, *, #2547, .F. ) ;
#6563 = DIRECTION ( 'NONE',  ( -8.326672684688674053E-17, 0.000000000000000000, -1.000000000000000000 ) ) ;
#6564 = CARTESIAN_POINT ( 'NONE',  ( 45.00000000000002132, -52.79999999999936477, 137.3500000000002217 ) ) ;
#6565 = LINE ( 'NONE', #4637, #17771 ) ;
#6566 = AXIS2_PLACEMENT_3D ( 'NONE', #15094, #22792, #13552 ) ;
#6567 = DIRECTION ( 'NONE',  ( -1.000000000000000000, -0.000000000000000000, -0.000000000000000000 ) ) ;
#6568 = CARTESIAN_POINT ( 'NONE',  ( 105.0000000000000000, -19.99999999999998934, 3.000000000000000000 ) ) ;
#6569 = DIRECTION ( 'NONE',  ( 3.469446951953614682E-16, -1.000000000000000000, 3.491481338843133355E-15 ) ) ;
#6570 = ADVANCED_FACE ( 'NONE', ( #17892 ), #23437, .T. ) ;
#6571 = ORIENTED_EDGE ( 'NONE', *, *, #21259, .F. ) ;
#6572 = LINE ( 'NONE', #13735, #2968 ) ;
#6573 = B_SPLINE_CURVE_WITH_KNOTS ( 'NONE', 3,
 ( #10823, #9098, #8984, #20081, #8875, #14666 ),
 .UNSPECIFIED., .F., .F.,
 ( 4, 2, 4 ),
 ( -3.640115492407174633E-06, 0.0002066546034006553863, 0.0004169493222937179812 ),
 .UNSPECIFIED. ) ;
#6574 = EDGE_CURVE ( 'NONE', #7513, #10936, #6905, .T. ) ;
#6575 = PRODUCT_DEFINITION_FORMATION_WITH_SPECIFIED_SOURCE ( 'ANY', '', #15766, .NOT_KNOWN. ) ;
#6576 = DIRECTION ( 'NONE',  ( 1.000000000000000000, 0.000000000000000000, -0.000000000000000000 ) ) ;
#6577 = CARTESIAN_POINT ( 'NONE',  ( 2.500000000000002220, 2.357898499370434386, -3.469446951953614189E-15 ) ) ;
#6578 = ITEM_DEFINED_TRANSFORMATION ( 'NONE', 'NONE', #13537,  #11210 ) ;
#6579 = VERTEX_POINT ( 'NONE', #6785 ) ;
#6580 = AXIS2_PLACEMENT_3D ( 'NONE', #801, #18112, #1902 ) ;
#6581 = VECTOR ( 'NONE', #21169, 1000.000000000000000 ) ;
#6582 = CARTESIAN_POINT ( 'NONE',  ( 70.00000000000000000, -87.33333333333332860, 3.000000000000000000 ) ) ;
#6583 = VERTEX_POINT ( 'NONE', #19699 ) ;
#6584 = DIRECTION ( 'NONE',  ( -0.000000000000000000, 0.8660254037844392627, 0.4999999999999990008 ) ) ;
#6585 = FACE_OUTER_BOUND ( 'NONE', #20085, .T. ) ;
#6586 = ORIENTED_EDGE ( 'NONE', *, *, #11316, .T. ) ;
#6587 = DIRECTION ( 'NONE',  ( 0.000000000000000000, 1.177509268541832635E-16, -1.000000000000000000 ) ) ;
#6588 = DIRECTION ( 'NONE',  ( 0.000000000000000000, 1.000000000000000000, -1.471414886128461471E-15 ) ) ;
#6589 = CARTESIAN_POINT ( 'NONE',  ( -282.2000000000008981, 35.00000000000100897, 102.3500000000000227 ) ) ;
#6590 = CARTESIAN_POINT ( 'NONE',  ( 281.4538215477169842, 269.4574776399289249, 145.6842353883612304 ) ) ;
#6591 = DIRECTION ( 'NONE',  ( -0.3090169943749370707, -0.9510565162951569729, 0.000000000000000000 ) ) ;
#6592 = PLANE ( 'NONE',  #22479 ) ;
#6593 = ORIENTED_EDGE ( 'NONE', *, *, #7220, .T. ) ;
#6594 = PRESENTATION_STYLE_ASSIGNMENT (( #2596 ) ) ;
#6595 = CARTESIAN_POINT ( 'NONE',  ( 145.9999999999998010, -799.0068695410399187, 30.00000000000641620 ) ) ;
#6596 = DIRECTION ( 'NONE',  ( 0.9289202219288174023, 0.3702799228849934510, 6.982962677686266711E-15 ) ) ;
#6597 = ORIENTED_EDGE ( 'NONE', *, *, #15972, .F. ) ;
#6598 = ADVANCED_FACE ( 'NONE', ( #17219 ), #1118, .T. ) ;
#6599 = VERTEX_POINT ( 'NONE', #19564 ) ;
#6600 = DIRECTION ( 'NONE',  ( 0.000000000000000000, -0.000000000000000000, -1.000000000000000000 ) ) ;
#6601 = EDGE_CURVE ( 'NONE', #4268, #22523, #4204, .T. ) ;
#6602 = FACE_OUTER_BOUND ( 'NONE', #18038, .T. ) ;
#6604 = DIRECTION ( 'NONE',  ( 1.000000000000000000, 0.000000000000000000, 0.000000000000000000 ) ) ;
#6603 = PRODUCT_DEFINITION_SHAPE ( 'NONE', 'NONE',  #23838 ) ;
#6605 = EDGE_CURVE ( 'NONE', #12563, #13397, #12396, .T. ) ;
#6606 = CARTESIAN_POINT ( 'NONE',  ( 132.6714475832642677, 80.14557597091010166, 32.48437713430730156 ) ) ;
#6607 = CARTESIAN_POINT ( 'NONE',  ( 2.700000000000001066, 0.000000000000000000, 0.000000000000000000 ) ) ;
#6608 = DIRECTION ( 'NONE',  ( -1.000000000000000000, -0.000000000000000000, -0.000000000000000000 ) ) ;
#6609 = ORIENTED_EDGE ( 'NONE', *, *, #12306, .T. ) ;
#6610 = CARTESIAN_POINT ( 'NONE',  ( -79.99999999999995737, -62.00000000000004263, 3.000000000000000000 ) ) ;
#6611 = DIRECTION ( 'NONE',  ( 0.000000000000000000, 0.000000000000000000, 1.000000000000000000 ) ) ;
#6612 = ADVANCED_FACE ( 'NONE', ( #19130, #6669 ), #12262, .F. ) ;
#6613 = LINE ( 'NONE', #1034, #1685 ) ;
#6614 = ORIENTED_EDGE ( 'NONE', *, *, #9386, .T. ) ;
#6615 = DIRECTION ( 'NONE',  ( -1.110223024625155594E-14, 0.000000000000000000, -1.000000000000000000 ) ) ;
#6616 = DIRECTION ( 'NONE',  ( 0.7071067811865416886, 0.000000000000000000, -0.7071067811865532349 ) ) ;
#6617 = DIRECTION ( 'NONE',  ( 0.000000000000000000, 0.000000000000000000, 1.000000000000000000 ) ) ;
#6618 = CARTESIAN_POINT ( 'NONE',  ( 3.266795293193171634, -1024.840023195373988, -145.0000000000001137 ) ) ;
#6619 = LINE ( 'NONE', #8665, #21134 ) ;
#6620 = DIRECTION ( 'NONE',  ( -0.000000000000000000, 1.000000000000000000, -3.469446951953613794E-15 ) ) ;
#6621 = CARTESIAN_POINT ( 'NONE',  ( -280.3431883566701686, 273.0000000000000568, 145.0627246244602304 ) ) ;
#6622 = ORIENTED_EDGE ( 'NONE', *, *, #21314, .F. ) ;
#6623 = VERTEX_POINT ( 'NONE', #3153 ) ;
#6624 = CARTESIAN_POINT ( 'NONE',  ( -280.4974534559950712, 269.7094021484634823, -146.1021437883072167 ) ) ;
#6625 = CARTESIAN_POINT ( 'NONE',  ( 280.8703180930666576, 269.1429506979392272, 146.7484459290826635 ) ) ;
#6626 = VERTEX_POINT ( 'NONE', #17349 ) ;
#6627 = LINE ( 'NONE', #14023, #16227 ) ;
#6628 = ORIENTED_EDGE ( 'NONE', *, *, #19934, .F. ) ;
#6629 = FACE_OUTER_BOUND ( 'NONE', #15566, .T. ) ;
#6630 = EDGE_CURVE ( 'NONE', #4114, #13072, #14064, .T. ) ;
#6631 = CARTESIAN_POINT ( 'NONE',  ( -126.4656051290186980, 89.61836744852057279, 30.32918505548581933 ) ) ;
#6632 = EDGE_LOOP ( 'NONE', ( #10079, #7008, #1628, #16428 ) ) ;
#6633 = EDGE_CURVE ( 'NONE', #13320, #9308, #16552, .T. ) ;
#6634 = DIRECTION ( 'NONE',  ( 0.000000000000000000, 0.000000000000000000, -1.000000000000000000 ) ) ;
#6635 = EDGE_LOOP ( 'NONE', ( #12150, #660 ) ) ;
#6636 = DIRECTION ( 'NONE',  ( -0.000000000000000000, -0.000000000000000000, 1.000000000000000000 ) ) ;
#6637 =( REPRESENTATION_RELATIONSHIP ('NONE','NONE', #10127, #4815 ) REPRESENTATION_RELATIONSHIP_WITH_TRANSFORMATION ( #11729 )SHAPE_REPRESENTATION_RELATIONSHIP( ) );
#6638 = EDGE_CURVE ( 'NONE', #20854, #13225, #3026, .T. ) ;
#6639 = DIRECTION ( 'NONE',  ( -1.000000000000000000, -0.000000000000000000, -0.000000000000000000 ) ) ;
#6640 = VERTEX_POINT ( 'NONE', #23567 ) ;
#6641 = ORIENTED_EDGE ( 'NONE', *, *, #18645, .F. ) ;
#6642 = CARTESIAN_POINT ( 'NONE',  ( -285.2000000000012960, -74.99999999999899103, -90.00000000000000000 ) ) ;
#6643 = EDGE_CURVE ( 'NONE', #10894, #15982, #795, .T. ) ;
#6644 = DIRECTION ( 'NONE',  ( 1.224646799147352468E-16, -1.848892746611745872E-32, 1.000000000000000000 ) ) ;
#6645 = CARTESIAN_POINT ( 'NONE',  ( 4.141042297810615835, -2.227970268150433863, -3.687027686973623819 ) ) ;
#6646 = DIRECTION ( 'NONE',  ( -0.000000000000000000, 1.000000000000000000, -3.469446951953613794E-15 ) ) ;
#6647 = DIRECTION ( 'NONE',  ( 0.000000000000000000, 0.000000000000000000, 1.000000000000000000 ) ) ;
#6648 = EDGE_CURVE ( 'NONE', #20079, #21672, #17340, .T. ) ;
#6649 = ORIENTED_EDGE ( 'NONE', *, *, #4432, .F. ) ;
#6650 = DIRECTION ( 'NONE',  ( -2.238759164535664589E-46, -3.469446951953614189E-15, -1.000000000000000000 ) ) ;
#6651 = ORIENTED_EDGE ( 'NONE', *, *, #20135, .T. ) ;
#6652 = ORIENTED_EDGE ( 'NONE', *, *, #22567, .T. ) ;
#6653 = FACE_OUTER_BOUND ( 'NONE', #5122, .T. ) ;
#6654 = ORIENTED_EDGE ( 'NONE', *, *, #5663, .F. ) ;
#6655 = DIRECTION ( 'NONE',  ( 0.000000000000000000, -1.000000000000000000, 0.000000000000000000 ) ) ;
#6656 = DIRECTION ( 'NONE',  ( 0.000000000000000000, 0.000000000000000000, 1.000000000000000000 ) ) ;
#6657 = ORIENTED_EDGE ( 'NONE', *, *, #10573, .T. ) ;
#6658 = EDGE_CURVE ( 'NONE', #18017, #9785, #7025, .T. ) ;
#6659 = LINE ( 'NONE', #14057, #21967 ) ;
#6660 = DIRECTION ( 'NONE',  ( 0.000000000000000000, -1.000000000000000000, -1.177509268541832635E-16 ) ) ;
#6661 = EDGE_CURVE ( 'NONE', #16285, #17916, #11817, .T. ) ;
#6662 = ORIENTED_EDGE ( 'NONE', *, *, #19583, .F. ) ;
#6663 = ADVANCED_FACE ( 'NONE', ( #12508 ), #4978, .T. ) ;
#6664 = CARTESIAN_POINT ( 'NONE',  ( -146.4450000000005332, -204.4690652294800657, -29.99999999999356248 ) ) ;
#6665 = EDGE_CURVE ( 'NONE', #12522, #18989, #8475, .T. ) ;
#6666 = CARTESIAN_POINT ( 'NONE',  ( 7.703928834700302986, -4.447865386531950627, -7.917997657324739258 ) ) ;
#6667 = DIRECTION ( 'NONE',  ( 0.000000000000000000, -0.000000000000000000, 1.000000000000000000 ) ) ;
#6668 = AXIS2_PLACEMENT_3D ( 'NONE', #12101, #6376, #14015 ) ;
#6669 = FACE_OUTER_BOUND ( 'NONE', #3565, .T. ) ;
#6670 = EDGE_CURVE ( 'NONE', #8689, #22922, #10900, .T. ) ;
#6671 = CARTESIAN_POINT ( 'NONE',  ( -7.500000000000000000, -4.330127018922199866, -1.000000000000000888 ) ) ;
#6672 = VERTEX_POINT ( 'NONE', #18354 ) ;
#6673 = DIRECTION ( 'NONE',  ( 0.000000000000000000, 0.000000000000000000, 1.000000000000000000 ) ) ;
#6674 = EDGE_CURVE ( 'NONE', #6350, #19296, #6542, .T. ) ;
#6676 = ORIENTED_EDGE ( 'NONE', *, *, #734, .T. ) ;
#6675 = ORIENTED_EDGE ( 'NONE', *, *, #18180, .F. ) ;
#6677 = DIRECTION ( 'NONE',  ( 0.000000000000000000, 0.000000000000000000, 1.000000000000000000 ) ) ;
#6678 = CARTESIAN_POINT ( 'NONE',  ( 0.000000000000000000, -129.2000000000000455, 7.690461757479017101E-15 ) ) ;
#6679 = FACE_OUTER_BOUND ( 'NONE', #2612, .T. ) ;
#6680 = DIRECTION ( 'NONE',  ( 0.000000000000000000, 0.000000000000000000, 1.000000000000000000 ) ) ;
#6681 = DIRECTION ( 'NONE',  ( -1.000000000000000000, -0.000000000000000000, -0.000000000000000000 ) ) ;
#6682 = CARTESIAN_POINT ( 'NONE',  ( 194.7500000000001990, -801.0618695410406644, -29.99999999999322498 ) ) ;
#6683 = ORIENTED_EDGE ( 'NONE', *, *, #17012, .F. ) ;
#6684 = VECTOR ( 'NONE', #10622, 1000.000000000000000 ) ;
#6685 = DIRECTION ( 'NONE',  ( 0.000000000000000000, 0.000000000000000000, -1.000000000000000000 ) ) ;
#6686 = ORIENTED_EDGE ( 'NONE', *, *, #149, .F. ) ;
#6687 = DIRECTION ( 'NONE',  ( 0.000000000000000000, -1.224646799147353454E-16, 1.000000000000000000 ) ) ;
#6688 = DIRECTION ( 'NONE',  ( -1.000000000000000000, 0.000000000000000000, 0.000000000000000000 ) ) ;
#6689 = ITEM_DEFINED_TRANSFORMATION ( 'NONE', 'NONE', #2281,  #11210 ) ;
#6690 = ORIENTED_EDGE ( 'NONE', *, *, #17142, .T. ) ;
#6691 = DIRECTION ( 'NONE',  ( 1.000000000000000000, 3.202566417187951028E-16, 6.405132834375902056E-16 ) ) ;
#6692 = EDGE_LOOP ( 'NONE', ( #14133, #15065, #8571, #3395 ) ) ;
#6693 = FACE_OUTER_BOUND ( 'NONE', #6722, .T. ) ;
#6694 = FACE_OUTER_BOUND ( 'NONE', #23503, .T. ) ;
#6695 = ORIENTED_EDGE ( 'NONE', *, *, #12887, .F. ) ;
#6696 = CARTESIAN_POINT ( 'NONE',  ( 102.3500000000000085, 35.00000000000000000, 3.000000000000001332 ) ) ;
#6697 = LINE ( 'NONE', #8632, #21508 ) ;
#6698 = AXIS2_PLACEMENT_3D ( 'NONE', #15481, #17272, #838 ) ;
#6699 = PRODUCT_DEFINITION_SHAPE ( 'NONE', 'NONE',  #23805 ) ;
#6700=STYLED_ITEM('',(#23913),#12677);
#6701 = LINE ( 'NONE', #4886, #7887 ) ;
#6702 = EDGE_CURVE ( 'NONE', #13026, #10799, #3440, .T. ) ;
#6703 = CARTESIAN_POINT ( 'NONE',  ( 281.1045205713626274, 269.7080393212557397, 145.4986342070537546 ) ) ;
#6704 = EDGE_CURVE ( 'NONE', #10742, #8313, #23110, .T. ) ;
#6705 = CARTESIAN_POINT ( 'NONE',  ( -285.2000000000013529, -89.99999999999896261, -40.33333333333332860 ) ) ;
#6706 = DIRECTION ( 'NONE',  ( -0.000000000000000000, 6.982962677686266711E-15, -1.000000000000000000 ) ) ;
#6707 = ORIENTED_EDGE ( 'NONE', *, *, #20259, .T. ) ;
#6708 = CYLINDRICAL_SURFACE ( 'NONE', #4933, 7.500000000000000888 ) ;
#6709 = DIRECTION ( 'NONE',  ( -0.000000000000000000, -0.000000000000000000, -1.000000000000000000 ) ) ;
#6710 = EDGE_LOOP ( 'NONE', ( #9697, #8958, #14457, #2955 ) ) ;
#6711 = ORIENTED_EDGE ( 'NONE', *, *, #16941, .T. ) ;
#6712 = LINE ( 'NONE', #21435, #8461 ) ;
#6713 = CARTESIAN_POINT ( 'NONE',  ( 34.55500000000001393, 0.000000000000000000, 0.000000000000000000 ) ) ;
#6714 = ADVANCED_BREP_SHAPE_REPRESENTATION ( '', ( #4039, #11210 ), #13515 ) ;
#6715 = CYLINDRICAL_SURFACE ( 'NONE', #2875, 5.249999999999973355 ) ;
#6716 = VECTOR ( 'NONE', #9768, 1000.000000000000000 ) ;
#6717 = VECTOR ( 'NONE', #12099, 1000.000000000000000 ) ;
#6718 = CARTESIAN_POINT ( 'NONE',  ( 4.154306624731035846, -2.398490048085128556, -3.721999068284417955 ) ) ;
#6719 = PLANE ( 'NONE',  #23487 ) ;
#6720 = EDGE_LOOP ( 'NONE', ( #18678, #12247, #11215, #14766, #7216 ) ) ;
#6721 = FACE_BOUND ( 'NONE', #6056, .T. ) ;
#6722 = EDGE_LOOP ( 'NONE', ( #20683, #6328, #4483, #17792 ) ) ;
#6723 = FACE_OUTER_BOUND ( 'NONE', #13226, .T. ) ;
#6724 = CARTESIAN_POINT ( 'NONE',  ( 5.000000000000004441, 0.000000000000000000, 0.000000000000000000 ) ) ;
#6725 =( NAMED_UNIT ( * ) SI_UNIT ( $, .STERADIAN. ) SOLID_ANGLE_UNIT ( ) );
#6726 = ORIENTED_EDGE ( 'NONE', *, *, #17526, .F. ) ;
#6727 = CARTESIAN_POINT ( 'NONE',  ( 4.000000000000000000, -2.309401076758514915, -3.433295621305383349 ) ) ;
#6728 = CYLINDRICAL_SURFACE ( 'NONE', #6865, 2.500000000000002220 ) ;
#6729 = DIRECTION ( 'NONE',  ( 0.000000000000000000, 0.000000000000000000, 1.000000000000000000 ) ) ;
#6730 = CARTESIAN_POINT ( 'NONE',  ( 19.87452195044109615, -1015.254575742277325, -145.0000000000001137 ) ) ;
#6731 = CARTESIAN_POINT ( 'NONE',  ( 45.00000000000000000, 272.9999999999999432, 0.000000000000000000 ) ) ;
#6732 = DIRECTION ( 'NONE',  ( 1.000000000000000000, 3.736327486719275871E-16, -1.296299001029869881E-30 ) ) ;
#6733 = FACE_OUTER_BOUND ( 'NONE', #12712, .T. ) ;
#6734 = VECTOR ( 'NONE', #2218, 1000.000000000000000 ) ;
#6735 = EDGE_LOOP ( 'NONE', ( #938, #154, #21324, #18695 ) ) ;
#6736 = CIRCLE ( 'NONE', #23304, 20.00000000000000000 ) ;
#6737 = VERTEX_POINT ( 'NONE', #12747 ) ;
#6738 = CARTESIAN_POINT ( 'NONE',  ( -10.00000000000000000, 1.224646799147353256E-15, -50.00000000000000000 ) ) ;
#6739 = CARTESIAN_POINT ( 'NONE',  ( -145.0000000000000284, -5.062647941322544249E-13, 90.00000000000000000 ) ) ;
#6740 = VERTEX_POINT ( 'NONE', #134 ) ;
#6741 = VECTOR ( 'NONE', #12249, 1000.000000000000000 ) ;
#6742 = CARTESIAN_POINT ( 'NONE',  ( 5.000000000000000000, 4.685197434473814759, -5.637851296924623057E-15 ) ) ;
#6743 = DIRECTION ( 'NONE',  ( 1.000000000000000000, 0.000000000000000000, 0.000000000000000000 ) ) ;
#6744 = ORIENTED_EDGE ( 'NONE', *, *, #18179, .T. ) ;
#6745 = CARTESIAN_POINT ( 'NONE',  ( -85.22886158240795851, -117.3074641843678876, -90.00000000000000000 ) ) ;
#6746 = DIRECTION ( 'NONE',  ( -0.000000000000000000, -0.000000000000000000, -1.000000000000000000 ) ) ;
#6747 = VERTEX_POINT ( 'NONE', #7248 ) ;
#6748 = CARTESIAN_POINT ( 'NONE',  ( -134.9759958199652203, -1076.200356551567211, -31.88744336596582940 ) ) ;
#6749 = CIRCLE ( 'NONE', #8688, 35.00000000000000711 ) ;
#6750 = VERTEX_POINT ( 'NONE', #7488 ) ;
#6751 = CARTESIAN_POINT ( 'NONE',  ( 0.000000000000000000, -1000.000000000000000, -138.9999999999999716 ) ) ;
#6752 = DIRECTION ( 'NONE',  ( 1.000000000000000000, 0.000000000000000000, 0.000000000000000000 ) ) ;
#6753 = ORIENTED_EDGE ( 'NONE', *, *, #17865, .T. ) ;
#6754 = ORIENTED_EDGE ( 'NONE', *, *, #8843, .T. ) ;
#6755 = CARTESIAN_POINT ( 'NONE',  ( 45.00000000000004974, -52.79999999999966320, 102.3500000000002075 ) ) ;
#6756 = VECTOR ( 'NONE', #859, 1000.000000000000000 ) ;
#6757 = DIRECTION ( 'NONE',  ( 1.000000000000000000, -3.495664435217746987E-15, 0.000000000000000000 ) ) ;
#6758 = AXIS2_PLACEMENT_3D ( 'NONE', #10420, #1326, #8708 ) ;
#6759 = CARTESIAN_POINT ( 'NONE',  ( -0.02448733951239248641, -4.877042772274742255, -3.751161874094027571 ) ) ;
#6760 = CARTESIAN_POINT ( 'NONE',  ( -4.406466114815342117, 6.116179640280717145, -7.446478553995464544 ) ) ;
#6761 = CARTESIAN_POINT ( 'NONE',  ( -160.0000000000000000, 0.000000000000000000, 90.00000000000000000 ) ) ;
#6762 = ADVANCED_FACE ( 'NONE', ( #5681 ), #1808, .F. ) ;
#6763 = VERTEX_POINT ( 'NONE', #20060 ) ;
#6764 = CARTESIAN_POINT ( 'NONE',  ( -194.7500000000005116, -204.4690652294793836, -32.49999999999322853 ) ) ;
#6765 = VECTOR ( 'NONE', #19203, 1000.000000000000114 ) ;
#6766 = EDGE_CURVE ( 'NONE', #21251, #18595, #3510, .T. ) ;
#6767 = EDGE_CURVE ( 'NONE', #4045, #2262, #7135, .T. ) ;
#6768 =( REPRESENTATION_RELATIONSHIP ('NONE','NONE', #10127, #4815 ) REPRESENTATION_RELATIONSHIP_WITH_TRANSFORMATION ( #8250 )SHAPE_REPRESENTATION_RELATIONSHIP( ) );
#6769 = VERTEX_POINT ( 'NONE', #1693 ) ;
#6770 = EDGE_CURVE ( 'NONE', #18600, #14720, #5489, .T. ) ;
#6771 = AXIS2_PLACEMENT_3D ( 'NONE', #10398, #17613, #4943 ) ;
#6772 = ORIENTED_EDGE ( 'NONE', *, *, #19801, .F. ) ;
#6773 = AXIS2_PLACEMENT_3D ( 'NONE', #21845, #20042, #3496 ) ;
#6774 = CARTESIAN_POINT ( 'NONE',  ( 90.00000000000000000, 3.000000000000293987, 129.9038105676659711 ) ) ;
#6775 = ORIENTED_EDGE ( 'NONE', *, *, #13795, .F. ) ;
#6776 = ORIENTED_EDGE ( 'NONE', *, *, #8577, .T. ) ;
#6777 = CONICAL_SURFACE ( 'NONE', #7936, 10.39117206796836079, 1.221730476396047926 ) ;
#6778 = CARTESIAN_POINT ( 'NONE',  ( -136.1034519145105719, -1074.167893320493249, 32.42079297023033035 ) ) ;
#6779 = CARTESIAN_POINT ( 'NONE',  ( 5.000000000000000000, 2.342598717236912709, 4.057499999999995666 ) ) ;
#6780 = EDGE_LOOP ( 'NONE', ( #12149, #17615 ) ) ;
#6781 = CONICAL_SURFACE ( 'NONE', #16422, 7.500000000000001776, 0.8594454914424796144 ) ;
#6782 = CARTESIAN_POINT ( 'NONE',  ( 0.000000000000000000, 0.000000000000000000, -90.00000000000000000 ) ) ;
#6783 = CARTESIAN_POINT ( 'NONE',  ( -280.2497115627123776, 269.9290760626064980, 145.5724317483736741 ) ) ;
#6784 =( NAMED_UNIT ( * ) SI_UNIT ( $, .STERADIAN. ) SOLID_ANGLE_UNIT ( ) );
#6785 = CARTESIAN_POINT ( 'NONE',  ( -127.9021285790837510, 87.55595642181940264, -27.49999999999351985 ) ) ;
#6786 = DIRECTION ( 'NONE',  ( 1.000000000000000000, 0.000000000000000000, 0.000000000000000000 ) ) ;
#6787 = ORIENTED_EDGE ( 'NONE', *, *, #9762, .F. ) ;
#6788 = CARTESIAN_POINT ( 'NONE',  ( -6.259644161404860030E-16, -4.618802153517027165, -3.433295621305388234 ) ) ;
#6789 = PRODUCT_DEFINITION_SHAPE ( 'NONE', 'NONE',  #23861 ) ;
#6790 = ADVANCED_FACE ( 'NONE', ( #7380 ), #9079, .F. ) ;
#6792 = ORIENTED_EDGE ( 'NONE', *, *, #16898, .F. ) ;
#6791 = EDGE_LOOP ( 'NONE', ( #11013, #141, #16761, #5142 ) ) ;
#6793 = CARTESIAN_POINT ( 'NONE',  ( 45.00000000000004263, -64.79999999999968452, 250.0000000000003411 ) ) ;
#6794 = CARTESIAN_POINT ( 'NONE',  ( -6.250000000000000888, 5.051814855409225480, -7.198902722707429369 ) ) ;
#6795 = VECTOR ( 'NONE', #16451, 1000.000000000000000 ) ;
#6796 = CARTESIAN_POINT ( 'NONE',  ( 2.500000000000000000, 1.178949249685212974, -2.042000000000001148 ) ) ;
#6797 = ADVANCED_FACE ( 'NONE', ( #14758 ), #19933, .F. ) ;
#6798 = FACE_OUTER_BOUND ( 'NONE', #501, .T. ) ;
#6799 = EDGE_CURVE ( 'NONE', #21081, #4308, #22825, .T. ) ;
#6800 = CARTESIAN_POINT ( 'NONE',  ( -281.3333820183296439, 269.5350371479512432, -145.6220388411722126 ) ) ;
#6801 = ORIENTED_EDGE ( 'NONE', *, *, #577, .F. ) ;
#6802 = CARTESIAN_POINT ( 'NONE',  ( 7.500000000000000000, -1.486698507076798847, -0.09861472150523931113 ) ) ;
#6803 = EDGE_CURVE ( 'NONE', #16727, #17822, #386, .T. ) ;
#6804 = EDGE_LOOP ( 'NONE', ( #4006, #18291, #11881 ) ) ;
#6805 = FACE_OUTER_BOUND ( 'NONE', #5952, .T. ) ;
#6806 = CONTEXT_DEPENDENT_SHAPE_REPRESENTATION ( #23712, #16065 ) ;
#6807 = VERTEX_POINT ( 'NONE', #2297 ) ;
#6808 = DIRECTION ( 'NONE',  ( 1.000000000000000000, 0.000000000000000000, 0.000000000000000000 ) ) ;
#6809 = ORIENTED_EDGE ( 'NONE', *, *, #1951, .T. ) ;
#6810 = CARTESIAN_POINT ( 'NONE',  ( -127.9949300873392275, 87.42039156791001631, -27.49999999999351985 ) ) ;
#6811 = DIRECTION ( 'NONE',  ( -1.000000000000000000, -0.000000000000000000, -0.000000000000000000 ) ) ;
#6812 = ORIENTED_EDGE ( 'NONE', *, *, #7300, .F. ) ;
#6813 = AXIS2_PLACEMENT_3D ( 'NONE', #18497, #15369, #9454 ) ;
#6814 = CARTESIAN_POINT ( 'NONE',  ( 281.4928932188134354, -127.0000000000000568, -150.2000000000013245 ) ) ;
#6815 = FACE_OUTER_BOUND ( 'NONE', #11889, .T. ) ;
#6816 = LINE ( 'NONE', #16006, #8271 ) ;
#6817 = LINE ( 'NONE', #14210, #13516 ) ;
#6818 = DIRECTION ( 'NONE',  ( -3.469446951953614682E-16, 1.000000000000000000, -3.483493295888648978E-15 ) ) ;
#6819 = CARTESIAN_POINT ( 'NONE',  ( 0.000000000000000000, 0.000000000000000000, -90.00000000000000000 ) ) ;
#6820 = VERTEX_POINT ( 'NONE', #13221 ) ;
#6821 = FACE_OUTER_BOUND ( 'NONE', #5643, .T. ) ;
#6822 = CARTESIAN_POINT ( 'NONE',  ( -4.000000000000000000, 0.8730739991738342143, -3.223134629628428893 ) ) ;
#6823 = ORIENTED_EDGE ( 'NONE', *, *, #3960, .T. ) ;
#6824 = ORIENTED_EDGE ( 'NONE', *, *, #23212, .F. ) ;
#6825 = PLANE ( 'NONE',  #15465 ) ;
#6826 = CARTESIAN_POINT ( 'NONE',  ( -5.000000000000001776, 0.000000000000000000, -9.974600000000000577 ) ) ;
#6827 = VECTOR ( 'NONE', #9675, 1000.000000000000000 ) ;
#6828 = CARTESIAN_POINT ( 'NONE',  ( -281.7350371479513456, 269.1333820183295416, 145.8708543776411659 ) ) ;
#6829 = ADVANCED_FACE ( 'NONE', ( #17045 ), #22457, .F. ) ;
#6830 = EDGE_CURVE ( 'NONE', #3824, #11791, #15128, .T. ) ;
#6831 = CARTESIAN_POINT ( 'NONE',  ( 5.000000000000000000, 5.258101095580057891E-15, 4.057499999999999218 ) ) ;
#6832 = ADVANCED_FACE ( 'NONE', ( #18951 ), #2414, .F. ) ;
#6833 = CARTESIAN_POINT ( 'NONE',  ( -282.3062614524588412, 272.4728700860325716, -145.4358181722190579 ) ) ;
#6834 = ORIENTED_EDGE ( 'NONE', *, *, #13697, .T. ) ;
#6835 = DIRECTION ( 'NONE',  ( -1.350636282998972974E-14, 0.000000000000000000, -1.000000000000000000 ) ) ;
#6836 = ORIENTED_EDGE ( 'NONE', *, *, #19483, .F. ) ;
#6837 = CARTESIAN_POINT ( 'NONE',  ( 40.00000000000000000, 100.0000000000000000, -125.0000000000000000 ) ) ;
#6838 = CARTESIAN_POINT ( 'NONE',  ( -146.0000000000000568, -494.4690652294807478, 32.05500000000641592 ) ) ;
#6839 = DIRECTION ( 'NONE',  ( 0.000000000000000000, 0.000000000000000000, -1.000000000000000000 ) ) ;
#6840 = ORIENTED_EDGE ( 'NONE', *, *, #23744, .T. ) ;
#6841 = AXIS2_PLACEMENT_3D ( 'NONE', #6852, #14253, #17727 ) ;
#6842 = CARTESIAN_POINT ( 'NONE',  ( 3.999999999999999112, -1.539600717839012978, -3.300726591567080703 ) ) ;
#6843 = CARTESIAN_POINT ( 'NONE',  ( 6.901579824520443829, -4.675625068323827627, -0.7022220667781372549 ) ) ;
#6844 = DIRECTION ( 'NONE',  ( 0.000000000000000000, -1.000000000000000000, 0.000000000000000000 ) ) ;
#6845 = CYLINDRICAL_SURFACE ( 'NONE', #9815, 2.649999999999985700 ) ;
#6847 = CIRCLE ( 'NONE', #17267, 2.055000000000000160 ) ;
#6846 = CARTESIAN_POINT ( 'NONE',  ( -2.699999999999995737, 0.000000000000000000, -20.30000000000000071 ) ) ;
#6848 = DIRECTION ( 'NONE',  ( -1.000000000000000000, -0.000000000000000000, -0.000000000000000000 ) ) ;
#6849 = FACE_OUTER_BOUND ( 'NONE', #17894, .T. ) ;
#6850 = EDGE_LOOP ( 'NONE', ( #8235, #17972, #10146, #15476 ) ) ;
#6851 = ORIENTED_EDGE ( 'NONE', *, *, #2940, .T. ) ;
#6852 = CARTESIAN_POINT ( 'NONE',  ( 0.000000000000000000, 0.000000000000000000, -90.00000000000000000 ) ) ;
#6853 = DIRECTION ( 'NONE',  ( 0.000000000000000000, 0.000000000000000000, 1.000000000000000000 ) ) ;
#6854 = VERTEX_POINT ( 'NONE', #11508 ) ;
#6855 = FACE_OUTER_BOUND ( 'NONE', #20374, .T. ) ;
#6856 = CARTESIAN_POINT ( 'NONE',  ( 16.55500000000001393, 0.000000000000000000, 0.000000000000000000 ) ) ;
#6857 = AXIS2_PLACEMENT_3D ( 'NONE', #6595, #22992, #5026 ) ;
#6858 = EDGE_LOOP ( 'NONE', ( #8619, #11601 ) ) ;
#6859 = CARTESIAN_POINT ( 'NONE',  ( 281.3684665479254932, 268.0880230824753312, 147.1999999999999886 ) ) ;
#6860 = DIRECTION ( 'NONE',  ( 0.000000000000000000, 0.000000000000000000, -1.000000000000000000 ) ) ;
#6861 = VERTEX_POINT ( 'NONE', #7857 ) ;
#6862 = EDGE_CURVE ( 'NONE', #16162, #12107, #16915, .T. ) ;
#6863 = CIRCLE ( 'NONE', #9478, 2.055000000000001492 ) ;
#6864 = CARTESIAN_POINT ( 'NONE',  ( -59.99999999999996447, -131.7994082814339833, 3.000000000000017764 ) ) ;
#6865 = AXIS2_PLACEMENT_3D ( 'NONE', #4917, #3101, #12457 ) ;
#6866 = CIRCLE ( 'NONE', #14582, 21.02499999999999503 ) ;
#6867 = VERTEX_POINT ( 'NONE', #20523 ) ;
#6868 = EDGE_CURVE ( 'NONE', #13320, #766, #7409, .T. ) ;
#6869 = LINE ( 'NONE', #22395, #4046 ) ;
#6870 = CARTESIAN_POINT ( 'NONE',  ( -285.2000000000006708, 90.00000000000100897, 32.35000000000001563 ) ) ;
#6871 = ORIENTED_EDGE ( 'NONE', *, *, #15712, .F. ) ;
#6872 = ORIENTED_EDGE ( 'NONE', *, *, #10521, .F. ) ;
#6873 = CARTESIAN_POINT ( 'NONE',  ( 133.8100684787067962, 78.22965734068039012, -31.65816015360256586 ) ) ;
#6874 = DIRECTION ( 'NONE',  ( 1.000000000000000000, -3.495664435217746987E-15, 0.000000000000000000 ) ) ;
#6875 = DIRECTION ( 'NONE',  ( 0.000000000000000000, 0.000000000000000000, 1.000000000000000000 ) ) ;
#6876 = CARTESIAN_POINT ( 'NONE',  ( -282.2000000000011255, -29.99999999999898037, -105.0000000000000000 ) ) ;
#6877 = LINE ( 'NONE', #23182, #4356 ) ;
#6878 = ORIENTED_EDGE ( 'NONE', *, *, #19409, .F. ) ;
#6879 = DIRECTION ( 'NONE',  ( 0.000000000000000000, -1.000000000000000000, 0.000000000000000000 ) ) ;
#6880 =( NAMED_UNIT ( * ) PLANE_ANGLE_UNIT ( ) SI_UNIT ( $, .RADIAN. ) );
#6881 = AXIS2_PLACEMENT_3D ( 'NONE', #6068, #7637, #11669 ) ;
#6882 = AXIS2_PLACEMENT_3D ( 'NONE', #18776, #5875, #4049 ) ;
#6883 = ORIENTED_EDGE ( 'NONE', *, *, #22437, .T. ) ;
#6884 = ADVANCED_FACE ( 'NONE', ( #12830 ), #7345, .T. ) ;
#6885 = ORIENTED_EDGE ( 'NONE', *, *, #23478, .T. ) ;
#6886 = LINE ( 'NONE', #14293, #22619 ) ;
#6887 = ORIENTED_EDGE ( 'NONE', *, *, #8978, .T. ) ;
#6888 = CARTESIAN_POINT ( 'NONE',  ( 0.2500000000000002220, 0.000000000000000000, 4.000000000000000000 ) ) ;
#6889 = VERTEX_POINT ( 'NONE', #7700 ) ;
#6890 = PRODUCT_DEFINITION_SHAPE ( 'NONE', 'NONE',  #20365 ) ;
#6891 = CIRCLE ( 'NONE', #21546, 2.649999999999999467 ) ;
#6892 = AXIS2_PLACEMENT_3D ( 'NONE', #6233, #2475, #18763 ) ;
#6893 = VECTOR ( 'NONE', #22524, 1000.000000000000000 ) ;
#6894 = LINE ( 'NONE', #2682, #6756 ) ;
#6895 = VECTOR ( 'NONE', #6323, 1000.000000000000000 ) ;
#6896 = ADVANCED_FACE ( 'NONE', ( #20598, #13053, #10887 ), #9291, .T. ) ;
#6897 = AXIS2_PLACEMENT_3D ( 'NONE', #18764, #7437, #86 ) ;
#6898 = EDGE_LOOP ( 'NONE', ( #20536, #8142, #6801, #8759 ) ) ;
#6899 = VECTOR ( 'NONE', #18977, 1000.000000000000000 ) ;
#6900 = DIRECTION ( 'NONE',  ( 0.000000000000000000, 0.000000000000000000, -1.000000000000000000 ) ) ;
#6901 = DIRECTION ( 'NONE',  ( 0.000000000000000000, -3.495664435217746987E-15, 1.000000000000000000 ) ) ;
#6902 = EDGE_CURVE ( 'NONE', #10962, #11798, #12866, .T. ) ;
#6903 = VECTOR ( 'NONE', #12316, 1000.000000000000000 ) ;
#6904 = FACE_OUTER_BOUND ( 'NONE', #15849, .T. ) ;
#6905 = LINE ( 'NONE', #2473, #20784 ) ;
#6906 = CARTESIAN_POINT ( 'NONE',  ( -140.0355749532208449, -37.61698748598668374, 90.00000000000000000 ) ) ;
#6907 = VERTEX_POINT ( 'NONE', #335 ) ;
#6908 = CARTESIAN_POINT ( 'NONE',  ( 50.00000000000000000, -59.80000000000001847, 2.159765843450962918E-13 ) ) ;
#6910 = ORIENTED_EDGE ( 'NONE', *, *, #14506, .F. ) ;
#6909 = ORIENTED_EDGE ( 'NONE', *, *, #16827, .F. ) ;
#6911 = VECTOR ( 'NONE', #16848, 1000.000000000000000 ) ;
#6913 = VECTOR ( 'NONE', #14898, 1000.000000000000000 ) ;
#6912 = CARTESIAN_POINT ( 'NONE',  ( -69.99999999999997158, -112.6666666666667282, 153.0000000000000000 ) ) ;
#6914 = AXIS2_PLACEMENT_3D ( 'NONE', #6946, #19730, #21669 ) ;
#6915 = DIRECTION ( 'NONE',  ( 0.000000000000000000, 0.000000000000000000, -1.000000000000000000 ) ) ;
#6916 = DIRECTION ( 'NONE',  ( 0.000000000000000000, 0.8660254037844380415, -0.5000000000000011102 ) ) ;
#6917 = AXIS2_PLACEMENT_3D ( 'NONE', #22153, #5749, #5624 ) ;
#6918 = CONICAL_SURFACE ( 'NONE', #9643, 4.057500000000000107, 1.047197551196593857 ) ;
#6919 = VECTOR ( 'NONE', #6037, 1000.000000000000000 ) ;
#6920 = CIRCLE ( 'NONE', #12372, 21.02499999999999503 ) ;
#6921 = CYLINDRICAL_SURFACE ( 'NONE', #16987, 5.249999999999942268 ) ;
#6922 = CARTESIAN_POINT ( 'NONE',  ( -155.0000000000000284, -204.4690652294799520, -29.99999999999350564 ) ) ;
#6923 = ORIENTED_EDGE ( 'NONE', *, *, #3127, .T. ) ;
#6924 = FACE_OUTER_BOUND ( 'NONE', #9225, .T. ) ;
#6925 = ORIENTED_EDGE ( 'NONE', *, *, #7030, .F. ) ;
#6926 = EDGE_CURVE ( 'NONE', #10443, #11094, #2126, .T. ) ;
#6927 = EDGE_CURVE ( 'NONE', #2147, #9524, #20246, .T. ) ;
#6928 = DIRECTION ( 'NONE',  ( 1.000000000000000000, 0.000000000000000000, 0.000000000000000000 ) ) ;
#6929 = CARTESIAN_POINT ( 'NONE',  ( -312.2000000000014666, -129.2000000000000455, 146.4928932188134638 ) ) ;
#6930 = EDGE_LOOP ( 'NONE', ( #8491, #13746, #532, #3183, #20332, #1922, #8276, #21726, #7195, #19956 ) ) ;
#6931 = ORIENTED_EDGE ( 'NONE', *, *, #20535, .F. ) ;
#6932 = CARTESIAN_POINT ( 'NONE',  ( -129.1746529357993722, 85.66745698985798185, -31.11299551804356156 ) ) ;
#6933 = CARTESIAN_POINT ( 'NONE',  ( -146.4450000000005048, -784.4690652294799520, -27.49999999999356604 ) ) ;
#6935 = AXIS2_PLACEMENT_3D ( 'NONE', #17335, #6584, #785 ) ;
#6934 = COLOUR_RGB ( '',1.000000000000000000, 0.9490196078431372140, 0.9098039215686274384 ) ;
#6936 = EDGE_LOOP ( 'NONE', ( #512, #21864 ) ) ;
#6937 = CARTESIAN_POINT ( 'NONE',  ( 5.000000000000004441, 0.000000000000000000, 0.000000000000000000 ) ) ;
#6938 = ADVANCED_FACE ( 'NONE', ( #22292 ), #16754, .F. ) ;
#6939 = CIRCLE ( 'NONE', #11620, 2.041999999999999815 ) ;
#6940 = DIRECTION ( 'NONE',  ( 1.000000000000000000, 0.000000000000000000, 0.000000000000000000 ) ) ;
#6941 = AXIS2_PLACEMENT_3D ( 'NONE', #16559, #27, #7378 ) ;
#6942 = AXIS2_PLACEMENT_3D ( 'NONE', #10985, #3467, #92 ) ;
#6943 = DIRECTION ( 'NONE',  ( 1.000000000000000000, -0.000000000000000000, -0.000000000000000000 ) ) ;
#6944 = EDGE_CURVE ( 'NONE', #13630, #3512, #11242, .T. ) ;
#6945 = CARTESIAN_POINT ( 'NONE',  ( 2.500000000000000000, 2.357898499370432166, -2.385244779468109755E-15 ) ) ;
#6946 = CARTESIAN_POINT ( 'NONE',  ( -69.99999999999997158, -112.6666666666667140, 144.9999999999999716 ) ) ;
#6947 = CARTESIAN_POINT ( 'NONE',  ( 3.750000000000004441, -6.495190528383289141, 0.000000000000000000 ) ) ;
#6948 = DIRECTION ( 'NONE',  ( 0.000000000000000000, 0.000000000000000000, 1.000000000000000000 ) ) ;
#6949 = EDGE_CURVE ( 'NONE', #21209, #8518, #7390, .T. ) ;
#6950 = ORIENTED_EDGE ( 'NONE', *, *, #10538, .F. ) ;
#6951 = CONTEXT_DEPENDENT_SHAPE_REPRESENTATION ( #12659, #2739 ) ;
#6952 = CARTESIAN_POINT ( 'NONE',  ( 155.0000000000000284, -500.0000000000000000, -29.99999999999997158 ) ) ;
#6953 = CARTESIAN_POINT ( 'NONE',  ( 7.894787914004607998, -0.7647108141804126458, -7.591390474663421095 ) ) ;
#6954 = EDGE_CURVE ( 'NONE', #4011, #10831, #2008, .T. ) ;
#6955 = ORIENTED_EDGE ( 'NONE', *, *, #23582, .F. ) ;
#6956 = DIRECTION ( 'NONE',  ( 1.000000000000000000, 0.000000000000000000, 0.000000000000000000 ) ) ;
#6957 = CARTESIAN_POINT ( 'NONE',  ( -79.99999999999995737, -56.80000000000006111, 2.099969703877781884E-13 ) ) ;
#6958 = AXIS2_PLACEMENT_3D ( 'NONE', #7498, #22219, #11041 ) ;
#6959 = AXIS2_PLACEMENT_3D ( 'NONE', #7930, #328, #4541 ) ;
#6960 = VECTOR ( 'NONE', #6485, 1000.000000000000114 ) ;
#6961 = CARTESIAN_POINT ( 'NONE',  ( -280.2880230824753198, 269.9999999999999432, 145.1244266708878570 ) ) ;
#6962 = DIRECTION ( 'NONE',  ( -2.775557561562891351E-17, 1.000000000000000000, 4.694093751100962712E-16 ) ) ;
#6963 = DIRECTION ( 'NONE',  ( 0.000000000000000000, 0.000000000000000000, 1.000000000000000000 ) ) ;
#6964 = ORIENTED_EDGE ( 'NONE', *, *, #8123, .F. ) ;
#6965 = DIRECTION ( 'NONE',  ( 0.000000000000000000, 0.000000000000000000, -1.000000000000000000 ) ) ;
#6966 = ORIENTED_EDGE ( 'NONE', *, *, #17747, .F. ) ;
#6967 = DIRECTION ( 'NONE',  ( 0.9289202219288174023, 0.3702799228849933955, 6.982962677686265922E-15 ) ) ;
#6968 = DIRECTION ( 'NONE',  ( 0.000000000000000000, 0.000000000000000000, 1.000000000000000000 ) ) ;
#6969 = EDGE_CURVE ( 'NONE', #9811, #5970, #1909, .T. ) ;
#6970 =( LENGTH_UNIT ( ) NAMED_UNIT ( * ) SI_UNIT ( .MILLI., .METRE. ) );
#6971 = EDGE_CURVE ( 'NONE', #6476, #14316, #18576, .T. ) ;
#6972 = EDGE_LOOP ( 'NONE', ( #18172, #22521, #9916, #21648 ) ) ;
#6973 = CARTESIAN_POINT ( 'NONE',  ( 65.00000000000001421, -56.79999999999939320, 125.0000000000002558 ) ) ;
#6974 = DIRECTION ( 'NONE',  ( -0.000000000000000000, 1.000000000000000000, 0.000000000000000000 ) ) ;
#6975 = CARTESIAN_POINT ( 'NONE',  ( -2.499999999999999556, -7.216878364870334295, -7.063244554130003294 ) ) ;
#6976 = CARTESIAN_POINT ( 'NONE',  ( -135.7895026000614109, -1074.740959209980247, 32.50000000000646594 ) ) ;
#6977 = AXIS2_PLACEMENT_3D ( 'NONE', #5212, #21751, #18015 ) ;
#6978 = EDGE_CURVE ( 'NONE', #1156, #17333, #16869, .T. ) ;
#6979 = DIRECTION ( 'NONE',  ( 0.000000000000000000, 0.7071067811865462405, -0.7071067811865489050 ) ) ;
#6980 = FACE_BOUND ( 'NONE', #14483, .T. ) ;
#6981 = CARTESIAN_POINT ( 'NONE',  ( -175.1609685624542863, -1088.719770019218458, -32.49999999999322853 ) ) ;
#6982 = VERTEX_POINT ( 'NONE', #7207 ) ;
#6983 = EDGE_CURVE ( 'NONE', #15719, #7318, #14016, .T. ) ;
#6984 = VERTEX_POINT ( 'NONE', #21946 ) ;
#6985 = CARTESIAN_POINT ( 'NONE',  ( -280.1255313583546354, 269.9999999999999432, -145.2905802150185366 ) ) ;
#6986 = LINE ( 'NONE', #20233, #21963 ) ;
#6987 = EDGE_CURVE ( 'NONE', #3347, #7088, #20133, .T. ) ;
#6988 = ORIENTED_EDGE ( 'NONE', *, *, #11292, .F. ) ;
#6989 = LINE ( 'NONE', #16165, #13114 ) ;
#6990 = LINE ( 'NONE', #1298, #2620 ) ;
#6991 = EDGE_LOOP ( 'NONE', ( #9027, #7737, #9844, #23326 ) ) ;
#6992 = CARTESIAN_POINT ( 'NONE',  ( 280.9952621458755289, 268.8927021017106540, 146.8958543268122128 ) ) ;
#6993 = CARTESIAN_POINT ( 'NONE',  ( 0.5984201754795568373, 8.314755988442765755, -0.7022220667781353676 ) ) ;
#6994 = ORIENTED_EDGE ( 'NONE', *, *, #1464, .T. ) ;
#6995 = CARTESIAN_POINT ( 'NONE',  ( -282.2000000000008981, 35.00000000000100897, 107.6499999999999631 ) ) ;
#6996 = EDGE_LOOP ( 'NONE', ( #945, #2595, #23581, #9753 ) ) ;
#6997 = DIRECTION ( 'NONE',  ( -2.775557561562891351E-17, 1.000000000000000000, -2.081668171172166936E-15 ) ) ;
#6998 = DIRECTION ( 'NONE',  ( -1.000000000000000000, 0.000000000000000000, -0.000000000000000000 ) ) ;
#6999 = CARTESIAN_POINT ( 'NONE',  ( 37.61698748598717401, -140.0355749532207312, -90.00000000000000000 ) ) ;
#7000 = ORIENTED_EDGE ( 'NONE', *, *, #11557, .F. ) ;
#7001 = EDGE_LOOP ( 'NONE', ( #6657, #10901 ) ) ;
#7002 = DIRECTION ( 'NONE',  ( -1.350636282998972974E-14, 0.000000000000000000, -1.000000000000000000 ) ) ;
#7003 = PRODUCT_DEFINITION_SHAPE ( 'NONE', 'NONE',  #23833 ) ;
#7004 = CARTESIAN_POINT ( 'NONE',  ( 40.00000000000000711, 100.0000000000000000, 114.9999999999999574 ) ) ;
#7005 = CARTESIAN_POINT ( 'NONE',  ( -127.9021285790837510, 87.55595642181941685, -32.49999999999351985 ) ) ;
#7006 = DIRECTION ( 'NONE',  ( -0.000000000000000000, -0.000000000000000000, 1.000000000000000000 ) ) ;
#7007 = CARTESIAN_POINT ( 'NONE',  ( 0.000000000000000000, 0.000000000000000000, 90.00000000000000000 ) ) ;
#7008 = ORIENTED_EDGE ( 'NONE', *, *, #8396, .T. ) ;
#7009 = EDGE_CURVE ( 'NONE', #12385, #6984, #10006, .T. ) ;
#7010 = CARTESIAN_POINT ( 'NONE',  ( 0.2500000000000002220, 4.898587196589412829E-16, -4.000000000000000000 ) ) ;
#7011 =( NAMED_UNIT ( * ) PLANE_ANGLE_UNIT ( ) SI_UNIT ( $, .RADIAN. ) );
#7012 = ADVANCED_FACE ( 'NONE', ( #9650 ), #2608, .F. ) ;
#7013 = ORIENTED_EDGE ( 'NONE', *, *, #21144, .T. ) ;
#7014 = EDGE_CURVE ( 'NONE', #23533, #3375, #20721, .T. ) ;
#7015 = DIRECTION ( 'NONE',  ( 0.000000000000000000, -0.000000000000000000, 1.000000000000000000 ) ) ;
#7016 = DIRECTION ( 'NONE',  ( -0.000000000000000000, -1.000000000000000000, -1.110223024625156540E-16 ) ) ;
#7017 = ORIENTED_EDGE ( 'NONE', *, *, #6053, .F. ) ;
#7018 = PLANE ( 'NONE',  #3673 ) ;
#7019 = ORIENTED_EDGE ( 'NONE', *, *, #16533, .F. ) ;
#7020 = LINE ( 'NONE', #20158, #8695 ) ;
#7021 = EDGE_LOOP ( 'NONE', ( #9205, #5001, #12000, #1000, #17116, #7424 ) ) ;
#7022 = DIRECTION ( 'NONE',  ( -1.000000000000000000, -0.000000000000000000, -0.000000000000000000 ) ) ;
#7023 = DIRECTION ( 'NONE',  ( -1.000000000000000000, 0.000000000000000000, 0.000000000000000000 ) ) ;
#7024 = DIRECTION ( 'NONE',  ( -1.000000000000000000, 0.000000000000000000, 0.000000000000000000 ) ) ;
#7025 = LINE ( 'NONE', #9863, #15814 ) ;
#7026 = DIRECTION ( 'NONE',  ( 3.736327486719275871E-16, -1.000000000000000000, 3.469446951953613794E-15 ) ) ;
#7027 = VERTEX_POINT ( 'NONE', #15564 ) ;
#7028 = DIRECTION ( 'NONE',  ( 0.000000000000000000, 0.000000000000000000, -1.000000000000000000 ) ) ;
#7029 = AXIS2_PLACEMENT_3D ( 'NONE', #11647, #6038, #18824 ) ;
#7030 = EDGE_CURVE ( 'NONE', #20231, #8518, #19274, .T. ) ;
#7032 = ORIENTED_EDGE ( 'NONE', *, *, #19897, .T. ) ;
#7031 = ORIENTED_EDGE ( 'NONE', *, *, #12434, .T. ) ;
#7033 = DIRECTION ( 'NONE',  ( 0.000000000000000000, 0.000000000000000000, 1.000000000000000000 ) ) ;
#7034 = DIRECTION ( 'NONE',  ( 0.000000000000000000, 5.551115123125777969E-15, -1.000000000000000000 ) ) ;
#7035 = CARTESIAN_POINT ( 'NONE',  ( 0.000000000000000000, 0.000000000000000000, 100.0000000000000000 ) ) ;
#7036 = ORIENTED_EDGE ( 'NONE', *, *, #13421, .F. ) ;
#7037 = DIRECTION ( 'NONE',  ( 1.000000000000000000, 0.000000000000000000, 0.000000000000000000 ) ) ;
#7038 = ORIENTED_EDGE ( 'NONE', *, *, #5488, .T. ) ;
#7039 = DIRECTION ( 'NONE',  ( 1.000000000000000000, -0.000000000000000000, -0.000000000000000000 ) ) ;
#7040 = ORIENTED_EDGE ( 'NONE', *, *, #15096, .T. ) ;
#7041 = DIRECTION ( 'NONE',  ( 6.580500949201931673E-15, 2.336402151923303105E-15, 1.000000000000000000 ) ) ;
#7042 = CARTESIAN_POINT ( 'NONE',  ( 5.000000000000000000, 4.685197434473814759, -5.637851296924623057E-15 ) ) ;
#7043 = ORIENTED_EDGE ( 'NONE', *, *, #11624, .F. ) ;
#7044 = CIRCLE ( 'NONE', #6668, 2.041999999999999815 ) ;
#7045 = ORIENTED_EDGE ( 'NONE', *, *, #10974, .F. ) ;
#7046 = DIRECTION ( 'NONE',  ( 0.000000000000000000, -0.000000000000000000, 1.000000000000000000 ) ) ;
#7047 = ORIENTED_EDGE ( 'NONE', *, *, #22555, .F. ) ;
#7048 = CARTESIAN_POINT ( 'NONE',  ( 0.000000000000000000, 0.000000000000000000, -9.974600000000000577 ) ) ;
#7049 = FACE_OUTER_BOUND ( 'NONE', #1110, .T. ) ;
#7050 = CARTESIAN_POINT ( 'NONE',  ( -146.0000000000001137, -494.4690652294807478, 27.94500000000641649 ) ) ;
#7051 = B_SPLINE_CURVE_WITH_KNOTS ( 'NONE', 3,
 ( #16602, #57, #16352, #11307, #11187, #19961, #18514, #1966 ),
 .UNSPECIFIED., .F., .F.,
 ( 4, 2, 2, 4 ),
 ( 0.000000000000000000, 0.002450665683189819262, 0.003675998524784728893, 0.004901331366379639391 ),
 .UNSPECIFIED. ) ;
#7052 = LINE ( 'NONE', #16714, #20006 ) ;
#7053 = CARTESIAN_POINT ( 'NONE',  ( 2.459698528280935825, -7.240146430416073642, -0.09933465333851955459 ) ) ;
#7054 = ORIENTED_EDGE ( 'NONE', *, *, #12443, .F. ) ;
#7055 = EDGE_CURVE ( 'NONE', #21142, #10685, #6124, .T. ) ;
#7056 = CARTESIAN_POINT ( 'NONE',  ( -7.500000000000000888, -1.443375672974068769, -7.063244554130002406 ) ) ;
#7057 = CARTESIAN_POINT ( 'NONE',  ( -3.436319922987618902, 2.634841920961291439, -3.531542292955721862 ) ) ;
#7058 = EDGE_CURVE ( 'NONE', #15352, #829, #17009, .T. ) ;
#7059 = ADVANCED_FACE ( 'NONE', ( #15674 ), #14391, .F. ) ;
#7060 = AXIS2_PLACEMENT_3D ( 'NONE', #19516, #21236, #19644 ) ;
#7061 = ORIENTED_EDGE ( 'NONE', *, *, #13329, .F. ) ;
#7062 = CYLINDRICAL_SURFACE ( 'NONE', #376, 5.200000000000031264 ) ;
#7063 = DIRECTION ( 'NONE',  ( -0.5000000000000008882, -0.8660254037844382635, 0.000000000000000000 ) ) ;
#7064 = EDGE_CURVE ( 'NONE', #18600, #6206, #19146, .T. ) ;
#7065 = CARTESIAN_POINT ( 'NONE',  ( -282.2000000000000455, 267.7999999999999545, 146.4928932188134354 ) ) ;
#7066 = CARTESIAN_POINT ( 'NONE',  ( 121.5574576620405622, -79.04925354955115324, -2.775557561562891351E-14 ) ) ;
#7067 = CARTESIAN_POINT ( 'NONE',  ( 194.7499999999997158, -801.0618695410399823, 32.50000000000675726 ) ) ;
#7068 = ORIENTED_EDGE ( 'NONE', *, *, #3848, .T. ) ;
#7070 = AXIS2_PLACEMENT_3D ( 'NONE', #22563, #20514, #7848 ) ;
#7069 = DIRECTION ( 'NONE',  ( -1.000000000000000000, 1.408839003528726857E-14, 6.982962677686266711E-15 ) ) ;
#7071 = ORIENTED_EDGE ( 'NONE', *, *, #2571, .T. ) ;
#7072 = DIRECTION ( 'NONE',  ( 0.000000000000000000, 0.000000000000000000, -1.000000000000000000 ) ) ;
#7074 = ADVANCED_FACE ( 'NONE', ( #4185 ), #6358, .T. ) ;
#7073 = DIRECTION ( 'NONE',  ( 0.000000000000000000, 0.000000000000000000, -1.000000000000000000 ) ) ;
#7075 = AXIS2_PLACEMENT_3D ( 'NONE', #11151, #20162, #11030 ) ;
#7076 = ORIENTED_EDGE ( 'NONE', *, *, #19966, .T. ) ;
#7077 = PLANE ( 'NONE',  #17749 ) ;
#7078 = CARTESIAN_POINT ( 'NONE',  ( 99.99999999999987210, -132.2000000000001023, 152.4000000000014268 ) ) ;
#7079 = LINE ( 'NONE', #19757, #19623 ) ;
#7080 = CARTESIAN_POINT ( 'NONE',  ( -44.99999999999997868, -52.79999999999938609, 140.0000000000001421 ) ) ;
#7081 = FACE_OUTER_BOUND ( 'NONE', #1382, .T. ) ;
#7082 = CARTESIAN_POINT ( 'NONE',  ( -130.4031948627971076, -44.80746418436799416, -90.00000000000000000 ) ) ;
#7083 = CARTESIAN_POINT ( 'NONE',  ( 158.0000000000000284, -500.0000000000000000, 27.35000000000002629 ) ) ;
#7084 = ORIENTED_EDGE ( 'NONE', *, *, #6239, .F. ) ;
#7085 = EDGE_LOOP ( 'NONE', ( #11423, #15351, #11328, #22585 ) ) ;
#7086 = DIRECTION ( 'NONE',  ( 0.000000000000000000, 0.000000000000000000, 1.000000000000000000 ) ) ;
#7087 = DIRECTION ( 'NONE',  ( 0.000000000000000000, 0.000000000000000000, 1.000000000000000000 ) ) ;
#7088 = VERTEX_POINT ( 'NONE', #20863 ) ;
#7089 = B_SPLINE_CURVE_WITH_KNOTS ( 'NONE', 3,
 ( #20373, #3492, #3841, #11257, #20146 ),
 .UNSPECIFIED., .F., .F.,
 ( 4, 1, 4 ),
 ( 0.000000000000000000, 0.002309401076758505356, 0.004618802153517010713 ),
 .UNSPECIFIED. ) ;
#7090 = AXIS2_PLACEMENT_3D ( 'NONE', #3483, #10892, #10760 ) ;
#7091 = PRODUCT_DEFINITION_SHAPE ( 'NONE', 'NONE',  #2813 ) ;
#7092 = CARTESIAN_POINT ( 'NONE',  ( 126.3653543294818178, 77.28387428943173632, -27.94499999999356632 ) ) ;
#7094 = TOROIDAL_SURFACE ( 'NONE', #12173, 22.50000000000000000, 1.500000000000000444 ) ;
#7093 = DIRECTION ( 'NONE',  ( -1.000000000000000000, 1.408839003528726857E-14, 6.982962677686266711E-15 ) ) ;
#7095 = ADVANCED_FACE ( 'NONE', ( #9882 ), #4341, .T. ) ;
#7096 = VERTEX_POINT ( 'NONE', #17239 ) ;
#7097 = CARTESIAN_POINT ( 'NONE',  ( 45.00000000000002132, -59.79999999999934346, 192.3500000000002785 ) ) ;
#7098 = ADVANCED_FACE ( 'NONE', ( #13408 ), #2375, .F. ) ;
#7099 = CARTESIAN_POINT ( 'NONE',  ( 119.9257125005557043, -1087.686723660050802, -29.99999999999356248 ) ) ;
#7100 = ORIENTED_EDGE ( 'NONE', *, *, #7660, .F. ) ;
#7101 = DIRECTION ( 'NONE',  ( -0.000000000000000000, 1.000000000000000000, -3.469446951953613794E-15 ) ) ;
#7102 = EDGE_CURVE ( 'NONE', #12825, #2537, #7420, .T. ) ;
#7103 = VERTEX_POINT ( 'NONE', #10126 ) ;
#7104 = CARTESIAN_POINT ( 'NONE',  ( 0.000000000000000000, 0.000000000000000000, 0.000000000000000000 ) ) ;
#7105 = ADVANCED_FACE ( 'NONE', ( #17118 ), #17473, .F. ) ;
#7106 = EDGE_CURVE ( 'NONE', #4691, #16783, #1624, .T. ) ;
#7107 = CARTESIAN_POINT ( 'NONE',  ( -7.499999999999999112, 41.99999999999998579, -100.0000000000000000 ) ) ;
#7108 = ORIENTED_EDGE ( 'NONE', *, *, #11631, .F. ) ;
#7109 = ORIENTED_EDGE ( 'NONE', *, *, #12162, .T. ) ;
#7110 = CARTESIAN_POINT ( 'NONE',  ( 284.1582675804705218, 270.9956429438695409, -145.8708543776411091 ) ) ;
#7111 =( NAMED_UNIT ( * ) PLANE_ANGLE_UNIT ( ) SI_UNIT ( $, .RADIAN. ) );
#7112 = DIRECTION ( 'NONE',  ( 0.000000000000000000, 0.000000000000000000, 1.000000000000000000 ) ) ;
#7113 = AXIS2_PLACEMENT_3D ( 'NONE', #22377, #14911, #7283 ) ;
#7114 = FACE_OUTER_BOUND ( 'NONE', #10569, .T. ) ;
#7115 = VECTOR ( 'NONE', #13049, 1000.000000000000000 ) ;
#7116 = DIRECTION ( 'NONE',  ( 0.000000000000000000, 1.000000000000000000, 0.000000000000000000 ) ) ;
#7117 = EDGE_LOOP ( 'NONE', ( #13046, #10761 ) ) ;
#7118 = CARTESIAN_POINT ( 'NONE',  ( -4.000000000000000000, 2.309401076758498483, -0.4999999999999927280 ) ) ;
#7119 = LINE ( 'NONE', #10780, #9855 ) ;
#7120 = LINE ( 'NONE', #14621, #1023 ) ;
#7121 = VECTOR ( 'NONE', #2153, 1000.000000000000000 ) ;
#7122 = VERTEX_POINT ( 'NONE', #6474 ) ;
#7123 = CARTESIAN_POINT ( 'NONE',  ( 0.000000000000000000, 0.000000000000000000, 0.000000000000000000 ) ) ;
#7124 = PRESENTATION_LAYER_ASSIGNMENT (  '', '', ( #10792 ) ) ;
#7125 = AXIS2_PLACEMENT_3D ( 'NONE', #2951, #8539, #12314 ) ;
#7126 = VERTEX_POINT ( 'NONE', #4054 ) ;
#7127 = EDGE_CURVE ( 'NONE', #748, #1699, #22653, .T. ) ;
#7128 = ADVANCED_FACE ( 'NONE', ( #4315 ), #955, .F. ) ;
#7129 = LINE ( 'NONE', #12738, #17166 ) ;
#7130 = ADVANCED_FACE ( 'NONE', ( #10161 ), #8581, .F. ) ;
#7131 = EDGE_LOOP ( 'NONE', ( #8931, #4459, #7234, #21617, #12795, #17739, #16675, #15139 ) ) ;
#7132 = DIRECTION ( 'NONE',  ( 0.000000000000000000, 0.000000000000000000, 1.000000000000000000 ) ) ;
#7133 = AXIS2_PLACEMENT_3D ( 'NONE', #19555, #6656, #9940 ) ;
#7134 = DIRECTION ( 'NONE',  ( -6.938893903907227392E-16, -1.000000000000000000, 0.000000000000000000 ) ) ;
#7135 = LINE ( 'NONE', #18239, #18220 ) ;
#7136 = DIRECTION ( 'NONE',  ( 0.000000000000000000, 0.000000000000000000, 1.000000000000000000 ) ) ;
#7137 = ORIENTED_EDGE ( 'NONE', *, *, #937, .T. ) ;
#7138 = DIRECTION ( 'NONE',  ( 0.5877852522924719159, 0.8090169943749482284, 0.000000000000000000 ) ) ;
#7139 = TOROIDAL_SURFACE ( 'NONE', #3658, 24.69999999999999929, 0.3000000000000007661 ) ;
#7141 = ORIENTED_EDGE ( 'NONE', *, *, #4932, .F. ) ;
#7140 = ORIENTED_EDGE ( 'NONE', *, *, #18407, .F. ) ;
#7142 = CARTESIAN_POINT ( 'NONE',  ( -293.2000000000010118, -89.99999999999963052, -40.33333333333406756 ) ) ;
#7143 = FACE_OUTER_BOUND ( 'NONE', #2052, .T. ) ;
#7144 = DIRECTION ( 'NONE',  ( 1.000000000000000000, 0.000000000000000000, 0.000000000000000000 ) ) ;
#7145 = ORIENTED_EDGE ( 'NONE', *, *, #7014, .F. ) ;
#7146 = DIRECTION ( 'NONE',  ( 1.000000000000000000, 0.000000000000000000, 0.000000000000000000 ) ) ;
#7147 = AXIS2_PLACEMENT_3D ( 'NONE', #9610, #192, #18633 ) ;
#7148 = DIRECTION ( 'NONE',  ( 0.000000000000000000, 0.000000000000000000, 1.000000000000000000 ) ) ;
#7149 = ORIENTED_EDGE ( 'NONE', *, *, #14358, .T. ) ;
#7150 = VECTOR ( 'NONE', #16082, 1000.000000000000000 ) ;
#7151 = DIRECTION ( 'NONE',  ( 0.000000000000000000, 0.000000000000000000, 1.000000000000000000 ) ) ;
#7152 = CARTESIAN_POINT ( 'NONE',  ( -1.118033988749894458, 0.000000000000000000, 0.000000000000000000 ) ) ;
#7153 = ITEM_DEFINED_TRANSFORMATION ( 'NONE', 'NONE', #22729,  #11210 ) ;
#7154 = ORIENTED_EDGE ( 'NONE', *, *, #3277, .F. ) ;
#7155 = AXIS2_PLACEMENT_3D ( 'NONE', #1832, #14546, #22013 ) ;
#7156 = ORIENTED_EDGE ( 'NONE', *, *, #10857, .F. ) ;
#7157 = FACE_OUTER_BOUND ( 'NONE', #22757, .T. ) ;
#7158 = ORIENTED_EDGE ( 'NONE', *, *, #23434, .T. ) ;
#7159 = LINE ( 'NONE', #3417, #6299 ) ;
#7160 = DIRECTION ( 'NONE',  ( 0.000000000000000000, 0.000000000000000000, 1.000000000000000000 ) ) ;
#7161 = DIRECTION ( 'NONE',  ( 0.000000000000000000, 0.000000000000000000, 1.000000000000000000 ) ) ;
#7162 = DIRECTION ( 'NONE',  ( 2.775557561562891351E-17, -1.000000000000000000, 0.000000000000000000 ) ) ;
#7163 = FACE_OUTER_BOUND ( 'NONE', #2890, .T. ) ;
#7164 = CIRCLE ( 'NONE', #17599, 2.500000000000000888 ) ;
#7165 = ORIENTED_EDGE ( 'NONE', *, *, #7872, .F. ) ;
#7166 =( NAMED_UNIT ( * ) SI_UNIT ( $, .STERADIAN. ) SOLID_ANGLE_UNIT ( ) );
#7167 = CARTESIAN_POINT ( 'NONE',  ( 0.000000000000000000, 0.000000000000000000, -150.0000000000000000 ) ) ;
#7168 = CARTESIAN_POINT ( 'NONE',  ( -100.0000000000001137, -127.0000000000000853, 147.2000000000013529 ) ) ;
#7169 = VERTEX_POINT ( 'NONE', #6761 ) ;
#7170 = CARTESIAN_POINT ( 'NONE',  ( 279.9999999999999432, 269.9999999999999432, -144.9999999999999716 ) ) ;
#7171 = CARTESIAN_POINT ( 'NONE',  ( -282.2000000000008981, 35.00000000000100897, 105.0000000000000000 ) ) ;
#7172 = ADVANCED_FACE ( 'NONE', ( #10414 ), #17870, .T. ) ;
#7173 = CARTESIAN_POINT ( 'NONE',  ( -285.0646579186753797, 269.1610889986682196, 146.2440776823445105 ) ) ;
#7174 = CARTESIAN_POINT ( 'NONE',  ( 2.500000000000000000, -1.178949249685218303, -2.041999999999998039 ) ) ;
#7175 = CARTESIAN_POINT ( 'NONE',  ( 280.4975000228325257, 272.3132312761074445, -147.6054396500289556 ) ) ;
#7176 = ORIENTED_EDGE ( 'NONE', *, *, #5917, .F. ) ;
#7177 = CARTESIAN_POINT ( 'NONE',  ( -280.0000000000000568, 272.9999999999999432, -144.9999999999999716 ) ) ;
#7178 = ORIENTED_EDGE ( 'NONE', *, *, #6830, .F. ) ;
#7179 = ADVANCED_FACE ( 'NONE', ( #8820 ), #19681, .F. ) ;
#7180 = DIRECTION ( 'NONE',  ( 0.000000000000000000, 0.000000000000000000, 1.000000000000000000 ) ) ;
#7181 = CARTESIAN_POINT ( 'NONE',  ( 0.000000000000000000, 0.000000000000000000, -4.974599999999998801 ) ) ;
#7182 = EDGE_CURVE ( 'NONE', #6529, #23723, #8600, .T. ) ;
#7183 = ORIENTED_EDGE ( 'NONE', *, *, #6246, .T. ) ;
#7184 = CARTESIAN_POINT ( 'NONE',  ( 2.500000000000000000, -1.178949249685214307, 2.042000000000001592 ) ) ;
#7185 = CARTESIAN_POINT ( 'NONE',  ( 123.3278826340502548, -1093.889547229276104, -31.65816015360254454 ) ) ;
#7186 = B_SPLINE_CURVE_WITH_KNOTS ( 'NONE', 3,
 ( #12686, #8796, #20228, #16157, #18082, #5507, #9272, #11092, #23517, #8926, #14470, #19997, #16633, #16385, #1535, #14372, #7324, #18300, #14710, #16499, #10980, #14826, #3461, #7193, #14581, #21923, #5400, #12817, #3564, #11335, #22773, #15432, #11704, #11583 ),
 .UNSPECIFIED., .F., .F.,
 ( 4, 2, 2, 2, 2, 2, 2, 2, 2, 2, 2, 2, 2, 2, 2, 2, 4 ),
 ( 0.000000000000000000, 0.03125000000000000694, 0.06250000000000000000, 0.09374999999999998612, 0.1249999999999999861, 0.1562499999999999722, 0.1874999999999999722, 0.2187500000000000000, 0.2500000000000000000, 0.2812500000000000000, 0.3125000000000000000, 0.3437500000000000000, 0.3750000000000000000, 0.4062500000000000555, 0.4375000000000000555, 0.4687500000000000555, 0.5000000000000000000 ),
 .UNSPECIFIED. ) ;
#7187 = CARTESIAN_POINT ( 'NONE',  ( 235.0000000000000284, -489.9999999999998863, 60.00000000000000000 ) ) ;
#7188 = CARTESIAN_POINT ( 'NONE',  ( 0.000000000000000000, -1.178949249685218748, -2.041999999999998039 ) ) ;
#7189 = LINE ( 'NONE', #1749, #1860 ) ;
#7190 = EDGE_CURVE ( 'NONE', #14046, #18754, #7826, .T. ) ;
#7191 = CARTESIAN_POINT ( 'NONE',  ( 3.000000000000002665, 0.000000000000000000, 0.000000000000000000 ) ) ;
#7192 = CIRCLE ( 'NONE', #6043, 145.0000000000000284 ) ;
#7193 = CARTESIAN_POINT ( 'NONE',  ( -15.24974479720507503, 19.87769063953886572, 145.0000119999999413 ) ) ;
#7194 = ORIENTED_EDGE ( 'NONE', *, *, #18849, .F. ) ;
#7195 = ORIENTED_EDGE ( 'NONE', *, *, #17095, .T. ) ;
#7196 = CARTESIAN_POINT ( 'NONE',  ( 70.00000000000000000, -112.6666666666666714, 124.9999999999999858 ) ) ;
#7197 = LINE ( 'NONE', #21816, #4630 ) ;
#7198 = VERTEX_POINT ( 'NONE', #17620 ) ;
#7199 = CYLINDRICAL_SURFACE ( 'NONE', #355, 5.199999999999982414 ) ;
#7200 = CARTESIAN_POINT ( 'NONE',  ( 4.419133455864432847, -6.108866147516184952, -7.026396753507086146 ) ) ;
#7201 = ORIENTED_EDGE ( 'NONE', *, *, #2066, .T. ) ;
#7202 = CIRCLE ( 'NONE', #13427, 2.649999999999971934 ) ;
#7203 = CARTESIAN_POINT ( 'NONE',  ( 279.9999999999999432, 269.9696999999999889, 145.0000000000000284 ) ) ;
#7204 = DIRECTION ( 'NONE',  ( 0.9289202219288174023, 0.3702799228849934510, 6.982962677686266711E-15 ) ) ;
#7205 = VERTEX_POINT ( 'NONE', #3244 ) ;
#7206 = CARTESIAN_POINT ( 'NONE',  ( 0.000000000000000000, 0.000000000000000000, -147.2000000000008981 ) ) ;
#7207 = CARTESIAN_POINT ( 'NONE',  ( -49.99999999999997158, -59.79999999999998295, 5.199999999999991296 ) ) ;
#7208 = AXIS2_PLACEMENT_3D ( 'NONE', #12340, #3214, #8432 ) ;
#7209 = APPLICATION_CONTEXT ( 'automotive_design' ) ;
#7210 = ORIENTED_EDGE ( 'NONE', *, *, #18932, .F. ) ;
#7211 = EDGE_CURVE ( 'NONE', #15403, #12940, #6877, .T. ) ;
#7212 = DIRECTION ( 'NONE',  ( -6.640089860198304064E-16, -1.000000000000000000, 0.000000000000000000 ) ) ;
#7213 = DIRECTION ( 'NONE',  ( 0.000000000000000000, 2.618450529776319755E-15, 1.000000000000000000 ) ) ;
#7214 = AXIS2_PLACEMENT_3D ( 'NONE', #12353, #21472, #19661 ) ;
#7215 = FACE_OUTER_BOUND ( 'NONE', #5457, .T. ) ;
#7216 = ORIENTED_EDGE ( 'NONE', *, *, #19679, .F. ) ;
#7217 = EDGE_LOOP ( 'NONE', ( #22701, #22158, #22464, #13916 ) ) ;
#7218 = FACE_OUTER_BOUND ( 'NONE', #21928, .T. ) ;
#7219 = DIRECTION ( 'NONE',  ( 0.000000000000000000, 1.000000000000000000, -1.103561164596346103E-15 ) ) ;
#7220 = EDGE_CURVE ( 'NONE', #16055, #6064, #21323, .T. ) ;
#7221 = CARTESIAN_POINT ( 'NONE',  ( 20.00000000000000000, 0.000000000000000000, -150.0000000000000000 ) ) ;
#7222 = CARTESIAN_POINT ( 'NONE',  ( 4.000000000000000000, -1.942223658245635809, -0.3516579909967643691 ) ) ;
#7223 = ADVANCED_FACE ( 'NONE', ( #8335 ), #5082, .F. ) ;
#7224 = ORIENTED_EDGE ( 'NONE', *, *, #3857, .F. ) ;
#7225 = CARTESIAN_POINT ( 'NONE',  ( -285.2000000000013529, -89.99999999999897682, 24.33333333333333215 ) ) ;
#7226 = AXIS2_PLACEMENT_3D ( 'NONE', #452, #15189, #9993 ) ;
#7227 = ADVANCED_FACE ( 'NONE', ( #10653, #17991 ), #14159, .F. ) ;
#7228 = PRODUCT_RELATED_PRODUCT_CATEGORY ( 'part', '', ( #12925 ) ) ;
#7229 = AXIS2_PLACEMENT_3D ( 'NONE', #22057, #773, #9155 ) ;
#7230 = EDGE_CURVE ( 'NONE', #10258, #8832, #20149, .T. ) ;
#7231 = CIRCLE ( 'NONE', #10756, 145.0000000000000284 ) ;
#7232 = DIRECTION ( 'NONE',  ( 0.000000000000000000, 0.000000000000000000, 1.000000000000000000 ) ) ;
#7233 = DIRECTION ( 'NONE',  ( -1.000000000000000000, 0.000000000000000000, 0.000000000000000000 ) ) ;
#7234 = ORIENTED_EDGE ( 'NONE', *, *, #10226, .F. ) ;
#7235 = DIRECTION ( 'NONE',  ( -0.7232617928448825673, 0.6905739489807055653, 6.982962677686266711E-15 ) ) ;
#7236 = EDGE_LOOP ( 'NONE', ( #21374, #41, #257, #15886 ) ) ;
#7237 = DIRECTION ( 'NONE',  ( -0.000000000000000000, -0.000000000000000000, 1.000000000000000000 ) ) ;
#7239 = VECTOR ( 'NONE', #3903, 1000.000000000000000 ) ;
#7238 = CARTESIAN_POINT ( 'NONE',  ( 5.000000000000000000, -2.342598717236900718, 4.057500000000001883 ) ) ;
#7240 = ORIENTED_EDGE ( 'NONE', *, *, #12890, .T. ) ;
#7241 = B_SPLINE_CURVE_WITH_KNOTS ( 'NONE', 3,
 ( #8686, #3227, #12112, #23035, #4701, #19408, #17495, #23404, #10395, #834, #14269, #21610, #3123, #6505, #2866, #4814, #19778, #17745, #8570, #17396, #15939, #6748, #8323, #16056, #944, #8448, #15702, #17609 ),
 .UNSPECIFIED., .F., .F.,
 ( 4, 2, 2, 2, 2, 2, 2, 2, 2, 2, 2, 2, 2, 4 ),
 ( 0.007862850516742094648, 0.008354729399060815617, 0.008846608281379538322, 0.009830366046016980261, 0.01032224492833550521, 0.01081412381065403015, 0.01130600269297255510, 0.01179788157529108178, 0.01278163933992811953, 0.01327351822224664274, 0.01376539710456516769, 0.01425727598688369263, 0.01474915486920221758, 0.01573291263383921890 ),
 .UNSPECIFIED. ) ;
#7242 = CARTESIAN_POINT ( 'NONE',  ( 7.499999999999997335, 34.18698582794336005, 100.0000000000000000 ) ) ;
#7243 = EDGE_CURVE ( 'NONE', #17692, #6740, #16195, .T. ) ;
#7244 = AXIS2_PLACEMENT_3D ( 'NONE', #10555, #16089, #18237 ) ;
#7245 = CARTESIAN_POINT ( 'NONE',  ( 24.99999999999998224, -1000.000000000000000, 145.0000059999999280 ) ) ;
#7246 = CONICAL_SURFACE ( 'NONE', #14617, 5.000000000000001776, 0.9599310885968795892 ) ;
#7247 = PLANE ( 'NONE',  #3772 ) ;
#7248 = CARTESIAN_POINT ( 'NONE',  ( -102.3500000000000227, -29.99999999999998579, 0.000000000000000000 ) ) ;
#7249 = AXIS2_PLACEMENT_3D ( 'NONE', #2738, #13763, #22998 ) ;
#7250 = CARTESIAN_POINT ( 'NONE',  ( 17.00000000000000000, 0.000000000000000000, 2.055000000000000160 ) ) ;
#7251 = ORIENTED_EDGE ( 'NONE', *, *, #6456, .T. ) ;
#7252 = EDGE_CURVE ( 'NONE', #18466, #22116, #19543, .T. ) ;
#7253 = DIRECTION ( 'NONE',  ( 1.000000000000000000, -0.000000000000000000, 0.000000000000000000 ) ) ;
#7255 = ORIENTED_EDGE ( 'NONE', *, *, #3539, .T. ) ;
#7254 = ORIENTED_EDGE ( 'NONE', *, *, #21281, .T. ) ;
#7256 = DIRECTION ( 'NONE',  ( 1.000000000000000000, 6.123233995736766036E-17, -6.123233995736764803E-17 ) ) ;
#7257 = EDGE_CURVE ( 'NONE', #2744, #4336, #4711, .T. ) ;
#7258 = DIRECTION ( 'NONE',  ( -4.625929269271485914E-16, 3.469446951953614583E-15, 1.000000000000000000 ) ) ;
#7259 = DIRECTION ( 'NONE',  ( 0.000000000000000000, 0.5000000000000011102, 0.8660254037844380415 ) ) ;
#7260 = ADVANCED_FACE ( 'NONE', ( #10536 ), #19314, .F. ) ;
#7261 = ORIENTED_EDGE ( 'NONE', *, *, #20979, .T. ) ;
#7262 = PRESENTATION_LAYER_ASSIGNMENT (  '', '', ( #10770 ) ) ;
#7263 = CYLINDRICAL_SURFACE ( 'NONE', #6427, 2.200000000000028155 ) ;
#7264 = CIRCLE ( 'NONE', #8064, 5.000000000000002665 ) ;
#7265 = CIRCLE ( 'NONE', #10007, 35.00000000000000711 ) ;
#7266 = CARTESIAN_POINT ( 'NONE',  ( 0.000000000000000000, 1.865214261513747767E-15, 138.9999999999999716 ) ) ;
#7267 = CIRCLE ( 'NONE', #17684, 5.200000000000028599 ) ;
#7268 = ORIENTED_EDGE ( 'NONE', *, *, #21842, .F. ) ;
#7269 = DIRECTION ( 'NONE',  ( -1.000000000000000000, 0.000000000000000000, -6.982962677686266711E-15 ) ) ;
#7270 = LINE ( 'NONE', #3632, #1887 ) ;
#7271 = AXIS2_PLACEMENT_3D ( 'NONE', #13776, #12321, #14006 ) ;
#7272 = CONTEXT_DEPENDENT_SHAPE_REPRESENTATION ( #2456, #6789 ) ;
#7273 = EDGE_LOOP ( 'NONE', ( #4842, #16571, #9538, #11746 ) ) ;
#7274 =( BOUNDED_SURFACE ( )  B_SPLINE_SURFACE ( 3, 2, ( 
 ( #2479, #22639, #20845 ),
 ( #4301, #3803, #7680 ),
 ( #9868, #16742, #22517 ),
 ( #17223, #15073, #673 ),
 ( #22279, #5754, #11452 ),
 ( #8050, #22407, #11228 ),
 ( #7803, #9384, #5867 ),
 ( #201, #15186, #13275 ) ),
 .UNSPECIFIED., .F., .F., .F. ) 
 B_SPLINE_SURFACE_WITH_KNOTS ( ( 4, 2, 2, 4 ),
 ( 3, 3 ),
 ( 0.03851319102641418551, 0.04314724750133520914, 0.04546427573879571749, 0.04778130397625623277 ),
 ( 0.000000000000000000, 1.000000000000000000 ),
 .UNSPECIFIED. ) 
 GEOMETRIC_REPRESENTATION_ITEM ( )  RATIONAL_B_SPLINE_SURFACE ( (
 ( 1.000000000000000000, 0.8047781573724569482, 1.000000000000000000),
 ( 1.000000000000000000, 0.8123768202405010630, 1.000000000000000000),
 ( 1.000000000000000000, 0.8190667609311549358, 1.000000000000000000),
 ( 1.000000000000000000, 0.8191933927154739781, 1.000000000000000000),
 ( 1.000000000000000000, 0.8176088169850088683, 1.000000000000000000),
 ( 1.000000000000000000, 0.8122958474542694152, 1.000000000000000000),
 ( 1.000000000000000000, 0.8086309703845098174, 1.000000000000000000),
 ( 1.000000000000000000, 0.8047712409910821041, 1.000000000000000000) ) ) 
 REPRESENTATION_ITEM ( '' )  SURFACE ( )  );
#7275 = ORIENTED_EDGE ( 'NONE', *, *, #22002, .F. ) ;
#7276 = CARTESIAN_POINT ( 'NONE',  ( 124.8578076529642971, -1091.845273256945802, 32.42126403526987133 ) ) ;
#7277 = VERTEX_POINT ( 'NONE', #12370 ) ;
#7278 = CARTESIAN_POINT ( 'NONE',  ( 19.87444003270859483, -984.7454789927647880, -145.0000000000001421 ) ) ;
#7279 = CARTESIAN_POINT ( 'NONE',  ( 158.0000000000000284, -500.0000000000000000, -29.99999999999997158 ) ) ;
#7280 = CARTESIAN_POINT ( 'NONE',  ( 4.250000000000000000, 0.000000000000000000, -10.00000000000000000 ) ) ;
#7281 = PRODUCT_DEFINITION_SHAPE ( 'NONE', 'NONE',  #7979 ) ;
#7282 = ADVANCED_FACE ( 'NONE', ( #2772 ), #113, .F. ) ;
#7283 = DIRECTION ( 'NONE',  ( 6.753181414994864868E-15, 0.000000000000000000, -1.000000000000000000 ) ) ;
#7285 = CIRCLE ( 'NONE', #20781, 2.649999999999985700 ) ;
#7284 =( GEOMETRIC_REPRESENTATION_CONTEXT ( 3 ) GLOBAL_UNCERTAINTY_ASSIGNED_CONTEXT ( ( #8 ) ) GLOBAL_UNIT_ASSIGNED_CONTEXT ( ( #17225, #11826, #19136 ) ) REPRESENTATION_CONTEXT ( 'NONE', 'WORKASPACE' ) );
#7286 = VECTOR ( 'NONE', #19741, 1000.000000000000000 ) ;
#7287 = LINE ( 'NONE', #10709, #10788 ) ;
#7288 = AXIS2_PLACEMENT_3D ( 'NONE', #11448, #13034, #9623 ) ;
#7289 = DIRECTION ( 'NONE',  ( 0.000000000000000000, 0.000000000000000000, 1.000000000000000000 ) ) ;
#7290 = VECTOR ( 'NONE', #4687, 1000.000000000000000 ) ;
#7291 = AXIS2_PLACEMENT_3D ( 'NONE', #9943, #517, #18723 ) ;
#7292 = AXIS2_PLACEMENT_3D ( 'NONE', #13452, #13809, #6404 ) ;
#7293 = ORIENTED_EDGE ( 'NONE', *, *, #2571, .F. ) ;
#7294 = DIRECTION ( 'NONE',  ( 0.000000000000000000, 0.000000000000000000, 1.000000000000000000 ) ) ;
#7295 = B_SPLINE_CURVE_WITH_KNOTS ( 'NONE', 3,
 ( #21015, #20522, #4474, #22697, #17405, #6171, #9922, #11879, #7856, #19187 ),
 .UNSPECIFIED., .F., .F.,
 ( 4, 2, 2, 2, 4 ),
 ( 0.000000000000000000, 0.002305503304226490767, 0.004611006608452981534, 0.006916509912679473168, 0.009222013216905964803 ),
 .UNSPECIFIED. ) ;
#7296 = EDGE_CURVE ( 'NONE', #23044, #4047, #1786, .T. ) ;
#7297 = FACE_OUTER_BOUND ( 'NONE', #40, .T. ) ;
#7298 = CARTESIAN_POINT ( 'NONE',  ( -4.175648173966055587, 2.207990556236529844, -3.469390959564062626 ) ) ;
#7299 = EDGE_LOOP ( 'NONE', ( #9302, #13594 ) ) ;
#7300 = EDGE_CURVE ( 'NONE', #3155, #18160, #16687, .T. ) ;
#7301 = CARTESIAN_POINT ( 'NONE',  ( -122.8605704798721803, 82.74225173005937961, -27.94499999999356632 ) ) ;
#7302 = CARTESIAN_POINT ( 'NONE',  ( -59.99999999999996447, -62.00000000000001421, 2.999999999999968914 ) ) ;
#7303 = CARTESIAN_POINT ( 'NONE',  ( -281.3689414351990763, 272.8938770989752811, 145.2488155364689248 ) ) ;
#7305 = CIRCLE ( 'NONE', #13910, 2.055000000000001492 ) ;
#7304 = AXIS2_PLACEMENT_3D ( 'NONE', #875, #5957, #15520 ) ;
#7306 = DIRECTION ( 'NONE',  ( 0.000000000000000000, 0.000000000000000000, 1.000000000000000000 ) ) ;
#7307 = DIRECTION ( 'NONE',  ( 1.000000000000000000, 0.000000000000000000, 0.000000000000000000 ) ) ;
#7308 = VECTOR ( 'NONE', #6459, 1000.000000000000000 ) ;
#7309 = AXIS2_PLACEMENT_3D ( 'NONE', #4869, #4744, #3045 ) ;
#7310 = ORIENTED_EDGE ( 'NONE', *, *, #5331, .F. ) ;
#7311 = CIRCLE ( 'NONE', #6941, 2.649999999999985700 ) ;
#7312 = VECTOR ( 'NONE', #9127, 1000.000000000000114 ) ;
#7313 = VECTOR ( 'NONE', #15694, 1000.000000000000000 ) ;
#7314 = DIRECTION ( 'NONE',  ( 0.000000000000000000, -1.224646799147353454E-16, 1.000000000000000000 ) ) ;
#7315 = ORIENTED_EDGE ( 'NONE', *, *, #19836, .F. ) ;
#7316 = CARTESIAN_POINT ( 'NONE',  ( -3.999999999999999112, 1.539600717838996324, -3.300726591567078039 ) ) ;
#7317 = CARTESIAN_POINT ( 'NONE',  ( 5.200000000000020606, 0.000000000000000000, -2.700000000000007727 ) ) ;
#7318 = VERTEX_POINT ( 'NONE', #16419 ) ;
#7319 = CARTESIAN_POINT ( 'NONE',  ( 122.9459112154324032, -1094.389103796012705, -29.83733181946741908 ) ) ;
#7320 = CARTESIAN_POINT ( 'NONE',  ( -5.007715329123872641E-16, -8.660254037844399733, -7.422398894150038728 ) ) ;
#7321 = DIRECTION ( 'NONE',  ( 0.000000000000000000, 0.000000000000000000, -1.000000000000000000 ) ) ;
#7322 = CARTESIAN_POINT ( 'NONE',  ( -45.24999999999994316, 100.0000000000000000, 147.2000000000005855 ) ) ;
#7323 = CARTESIAN_POINT ( 'NONE',  ( 2.700000000000001510, 0.000000000000000000, -24.69999999999999929 ) ) ;
#7324 = CARTESIAN_POINT ( 'NONE',  ( 1.636246173744676291, 24.99999999999999645, 145.0000119999999697 ) ) ;
#7325 = EDGE_LOOP ( 'NONE', ( #13993, #18651, #14101, #21159, #8342 ) ) ;
#7326 = VERTEX_POINT ( 'NONE', #14856 ) ;
#7327 = AXIS2_PLACEMENT_3D ( 'NONE', #18362, #3518, #16573 ) ;
#7328 = CARTESIAN_POINT ( 'NONE',  ( 1.655952806101427033, -3.662737355149048302, -1.182683869819604841E-14 ) ) ;
#7329 = CARTESIAN_POINT ( 'NONE',  ( -130.4031948627974486, 44.80746418436699940, -90.00000000000000000 ) ) ;
#7330 = VECTOR ( 'NONE', #2681, 1000.000000000000114 ) ;
#7331 = AXIS2_PLACEMENT_3D ( 'NONE', #10687, #23576, #8974 ) ;
#7332 = ORIENTED_EDGE ( 'NONE', *, *, #9354, .F. ) ;
#7333 = AXIS2_PLACEMENT_3D ( 'NONE', #21639, #19694, #18010 ) ;
#7334 = AXIS2_PLACEMENT_3D ( 'NONE', #4775, #12186, #16015 ) ;
#7335 = EDGE_CURVE ( 'NONE', #19715, #1314, #6277, .T. ) ;
#7336 = ADVANCED_FACE ( 'NONE', ( #11127, #16532, #18117, #14499, #23655 ), #5538, .T. ) ;
#7337 = LINE ( 'NONE', #9152, #19287 ) ;
#7338 = DIRECTION ( 'NONE',  ( 1.000000000000000000, 0.000000000000000000, 0.000000000000000000 ) ) ;
#7339 = ORIENTED_EDGE ( 'NONE', *, *, #19678, .T. ) ;
#7340 = CARTESIAN_POINT ( 'NONE',  ( 280.6220388411721274, 269.5350371479512432, 146.3333820183295586 ) ) ;
#7341 = CARTESIAN_POINT ( 'NONE',  ( 30.00000000000000000, 0.000000000000000000, -6.938893903907228378E-15 ) ) ;
#7342 = ORIENTED_EDGE ( 'NONE', *, *, #6638, .F. ) ;
#7343 = FACE_BOUND ( 'NONE', #21964, .T. ) ;
#7344 = EDGE_CURVE ( 'NONE', #5348, #2405, #14397, .T. ) ;
#7345 = CYLINDRICAL_SURFACE ( 'NONE', #12487, 4.250000000000000000 ) ;
#7346 = CARTESIAN_POINT ( 'NONE',  ( 0.000000000000000000, 0.000000000000000000, 100.0000000000000000 ) ) ;
#7347 = EDGE_LOOP ( 'NONE', ( #8413, #21734 ) ) ;
#7348 = PLANE ( 'NONE',  #7612 ) ;
#7349 = DIRECTION ( 'NONE',  ( -1.000000000000000000, -3.469446951953627008E-16, -3.469446951953616161E-16 ) ) ;
#7350 = VECTOR ( 'NONE', #3513, 1000.000000000000000 ) ;
#7351 = CARTESIAN_POINT ( 'NONE',  ( 287.4000000000013415, -127.0000000000000568, -146.4928932188134070 ) ) ;
#7352 = ORIENTED_EDGE ( 'NONE', *, *, #835, .T. ) ;
#7353 = ORIENTED_EDGE ( 'NONE', *, *, #16566, .T. ) ;
#7354 = CARTESIAN_POINT ( 'NONE',  ( -282.2000000000013529, -89.99999999999897682, 24.33333333333333215 ) ) ;
#7355 = AXIS2_PLACEMENT_3D ( 'NONE', #1286, #2751, #17481 ) ;
#7356 = TOROIDAL_SURFACE ( 'NONE', #10854, 24.69999999999999929, 0.3000000000000007661 ) ;
#7357 = PRODUCT_CONTEXT ( 'NONE', #6135, 'mechanical' ) ;
#7358 = CARTESIAN_POINT ( 'NONE',  ( -126.7571989378447910, 89.20549877611344414, -28.46977261728505937 ) ) ;
#7359 = CARTESIAN_POINT ( 'NONE',  ( -7.848314987057850800, 4.129027267381560229, -7.493854785173809319 ) ) ;
#7360 = CARTESIAN_POINT ( 'NONE',  ( 45.24999999999994316, 100.0000000000000000, -150.2000000000005571 ) ) ;
#7361 = ORIENTED_EDGE ( 'NONE', *, *, #14479, .F. ) ;
#7362 = CARTESIAN_POINT ( 'NONE',  ( -44.99999999999995026, -52.79999999999970584, 47.35000000000019327 ) ) ;
#7363 = EDGE_CURVE ( 'NONE', #12, #1352, #16885, .T. ) ;
#7364 = UNCERTAINTY_MEASURE_WITH_UNIT (LENGTH_MEASURE( 1.000000000000000082E-05 ), #18518, 'distance_accuracy_value', 'NONE');
#7365 = APPLICATION_CONTEXT ( 'automotive_design' ) ;
#7366 = LINE ( 'NONE', #16424, #22164 ) ;
#7367 = DIRECTION ( 'NONE',  ( 1.000000000000000000, -0.000000000000000000, 6.982962677686266711E-15 ) ) ;
#7368 = EDGE_LOOP ( 'NONE', ( #10750, #10550 ) ) ;
#7369 = CARTESIAN_POINT ( 'NONE',  ( -122.8605704798721945, 82.74225173005939382, -29.99999999999356604 ) ) ;
#7370 = ADVANCED_FACE ( 'NONE', ( #22186 ), #21836, .F. ) ;
#7371 = EDGE_CURVE ( 'NONE', #13555, #2034, #8952, .T. ) ;
#7372 = VERTEX_POINT ( 'NONE', #16658 ) ;
#7373 = CARTESIAN_POINT ( 'NONE',  ( 17.00000000000000000, 2.055000000000000160, 0.000000000000000000 ) ) ;
#7374 = CARTESIAN_POINT ( 'NONE',  ( 2.428612866367495853E-14, 35.00000000000002842, 150.2000000000008413 ) ) ;
#7375 = ORIENTED_EDGE ( 'NONE', *, *, #4292, .T. ) ;
#7376 = CARTESIAN_POINT ( 'NONE',  ( -129.2722218393572859, 85.52013646629116295, -29.34624901867147528 ) ) ;
#7377 = EDGE_CURVE ( 'NONE', #2834, #13773, #5658, .T. ) ;
#7378 = DIRECTION ( 'NONE',  ( 0.000000000000000000, 1.000000000000000000, 0.000000000000000000 ) ) ;
#7379 = DIRECTION ( 'NONE',  ( 3.736327486719275871E-16, -1.000000000000000000, 3.469446951953614189E-15 ) ) ;
#7380 = FACE_OUTER_BOUND ( 'NONE', #11625, .T. ) ;
#7381 = DIRECTION ( 'NONE',  ( 0.000000000000000000, 0.000000000000000000, 1.000000000000000000 ) ) ;
#7382 = ORIENTED_EDGE ( 'NONE', *, *, #7713, .F. ) ;
#7383 = LINE ( 'NONE', #5334, #7350 ) ;
#7384 = PLANE ( 'NONE',  #12520 ) ;
#7386 = VERTEX_POINT ( 'NONE', #7360 ) ;
#7385 = ORIENTED_EDGE ( 'NONE', *, *, #15510, .T. ) ;
#7387 = DIRECTION ( 'NONE',  ( 0.000000000000000000, 0.000000000000000000, 1.000000000000000000 ) ) ;
#7388 = CARTESIAN_POINT ( 'NONE',  ( -6.127431526422343306E-17, 9.147862274876549904, -8.047472243342932430 ) ) ;
#7389 = CARTESIAN_POINT ( 'NONE',  ( 279.9999999999999432, 269.9697000000000457, -144.9999999999999716 ) ) ;
#7390 = B_SPLINE_CURVE_WITH_KNOTS ( 'NONE', 3,
 ( #4086, #5524, #16646, #9159, #18554, #14726, #3696, #11348 ),
 .UNSPECIFIED., .F., .F.,
 ( 4, 2, 2, 4 ),
 ( 0.005725059856848641743, 0.006314084072593626612, 0.006903108288338611481, 0.008081156719828581220 ),
 .UNSPECIFIED. ) ;
#7391 = ORIENTED_EDGE ( 'NONE', *, *, #1724, .T. ) ;
#7392 = DIRECTION ( 'NONE',  ( 0.000000000000000000, 1.000000000000000000, -3.548298019043423769E-15 ) ) ;
#7393 = ORIENTED_EDGE ( 'NONE', *, *, #1470, .F. ) ;
#7394 = EDGE_CURVE ( 'NONE', #2833, #1592, #5118, .T. ) ;
#7395 = CARTESIAN_POINT ( 'NONE',  ( 0.000000000000000000, 0.000000000000000000, -10.00000000000000000 ) ) ;
#7396 = EDGE_CURVE ( 'NONE', #5897, #18021, #7089, .T. ) ;
#7397 = ORIENTED_EDGE ( 'NONE', *, *, #271, .T. ) ;
#7398 = EDGE_CURVE ( 'NONE', #12588, #3415, #14612, .T. ) ;
#7399 = CARTESIAN_POINT ( 'NONE',  ( -31.74999999999995737, 0.000000000000000000, 2.500000000000000444 ) ) ;
#7400 = DIRECTION ( 'NONE',  ( 3.736327486719275871E-16, -1.000000000000000000, 3.469446951953614189E-15 ) ) ;
#7401 = ORIENTED_EDGE ( 'NONE', *, *, #13896, .T. ) ;
#7402 = EDGE_CURVE ( 'NONE', #15759, #7620, #10899, .T. ) ;
#7403 = CARTESIAN_POINT ( 'NONE',  ( 125.5963796795001031, -1090.832610870656481, 28.34264858295336964 ) ) ;
#7404 = ORIENTED_EDGE ( 'NONE', *, *, #20190, .F. ) ;
#7405 =( REPRESENTATION_RELATIONSHIP ('NONE','NONE', #10127, #6236 ) REPRESENTATION_RELATIONSHIP_WITH_TRANSFORMATION ( #3891 )SHAPE_REPRESENTATION_RELATIONSHIP( ) );
#7406 = EDGE_CURVE ( 'NONE', #23584, #7027, #14739, .T. ) ;
#7407 = CARTESIAN_POINT ( 'NONE',  ( -128.9689330775211999, 85.97690438148575254, 28.34264858295340517 ) ) ;
#7408 = DIRECTION ( 'NONE',  ( -0.000000000000000000, -0.000000000000000000, 1.000000000000000000 ) ) ;
#7409 = CIRCLE ( 'NONE', #5103, 7.499999999999996447 ) ;
#7410 = CARTESIAN_POINT ( 'NONE',  ( 4.000000000000000000, -2.511475576507276042, -3.469253905236643565 ) ) ;
#7411 = CARTESIAN_POINT ( 'NONE',  ( 40.00000000000000000, 100.0000000000000000, 145.0000000000000000 ) ) ;
#7412 = CARTESIAN_POINT ( 'NONE',  ( -282.2000000000012960, -74.99999999999899103, -90.00000000000000000 ) ) ;
#7413 = CONTEXT_DEPENDENT_SHAPE_REPRESENTATION ( #2272, #10089 ) ;
#7414 = EDGE_LOOP ( 'NONE', ( #10826, #14587 ) ) ;
#7415 = CARTESIAN_POINT ( 'NONE',  ( 2.500000000000000000, -1.178949249685213863, 2.042000000000001148 ) ) ;
#7416 = CARTESIAN_POINT ( 'NONE',  ( 6.874999999999997335, -4.690970937165716670, -7.298562697733105509 ) ) ;
#7417 = ORIENTED_EDGE ( 'NONE', *, *, #3802, .F. ) ;
#7418 = DIRECTION ( 'NONE',  ( 1.000000000000000000, -3.495664435217746987E-15, -0.000000000000000000 ) ) ;
#7419 = FACE_OUTER_BOUND ( 'NONE', #16199, .T. ) ;
#7420 = CIRCLE ( 'NONE', #12102, 2.500000000000000444 ) ;
#7421 = CARTESIAN_POINT ( 'NONE',  ( 7.500000000000000888, 1.489914625144004523, -0.1187923833806749097 ) ) ;
#7422 = DIRECTION ( 'NONE',  ( -1.000000000000000000, 1.408839003528726857E-14, 6.982962677686266711E-15 ) ) ;
#7423 = CARTESIAN_POINT ( 'NONE',  ( -281.6810649015078525, 272.7324007871372942, -145.3120962995436116 ) ) ;
#7424 = ORIENTED_EDGE ( 'NONE', *, *, #22404, .F. ) ;
#7425 = CARTESIAN_POINT ( 'NONE',  ( 11.07878015919986048, -977.5291759891807715, 145.0000119999999697 ) ) ;
#7426 = EDGE_LOOP ( 'NONE', ( #12854, #11638 ) ) ;
#7427 = CARTESIAN_POINT ( 'NONE',  ( -285.2000000000010118, 9.892604858775022387E-13, -146.4928932188134070 ) ) ;
#7428 = DIRECTION ( 'NONE',  ( 1.000000000000000000, 0.000000000000000000, -0.000000000000000000 ) ) ;
#7429 = EDGE_CURVE ( 'NONE', #13361, #4420, #18333, .T. ) ;
#7430 = ADVANCED_FACE ( 'NONE', ( #2505 ), #13564, .F. ) ;
#7431 = CARTESIAN_POINT ( 'NONE',  ( 155.0000000000000284, -500.0000000000000000, -27.34999999999998721 ) ) ;
#7432 = ORIENTED_EDGE ( 'NONE', *, *, #15684, .T. ) ;
#7433 = CARTESIAN_POINT ( 'NONE',  ( 5.200000000000002842, 0.000000000000000000, -2.700000000000000622 ) ) ;
#7434 = CARTESIAN_POINT ( 'NONE',  ( -69.99999999999997158, -112.6666666666667140, 0.000000000000000000 ) ) ;
#7435 = CARTESIAN_POINT ( 'NONE',  ( 235.0000000000000284, -557.0000000000000000, -57.00000000000000000 ) ) ;
#7436 = FACE_BOUND ( 'NONE', #7426, .T. ) ;
#7437 = DIRECTION ( 'NONE',  ( -0.000000000000000000, -0.000000000000000000, 1.000000000000000000 ) ) ;
#7438 = DIRECTION ( 'NONE',  ( 0.000000000000000000, 0.000000000000000000, -1.000000000000000000 ) ) ;
#7439 = ORIENTED_EDGE ( 'NONE', *, *, #1857, .T. ) ;
#7440 = ORIENTED_EDGE ( 'NONE', *, *, #12332, .F. ) ;
#7441 = DIRECTION ( 'NONE',  ( 0.000000000000000000, 0.000000000000000000, 1.000000000000000000 ) ) ;
#7442 = DIRECTION ( 'NONE',  ( 1.000000000000000000, 0.000000000000000000, 0.000000000000000000 ) ) ;
#7443 = ORIENTED_EDGE ( 'NONE', *, *, #12162, .F. ) ;
#7444 = DIRECTION ( 'NONE',  ( 0.000000000000000000, 0.000000000000000000, -1.000000000000000000 ) ) ;
#7445 = CARTESIAN_POINT ( 'NONE',  ( -0.04606493828583551470, -9.175055303659563677, -8.057411785091794343 ) ) ;
#7446 = CARTESIAN_POINT ( 'NONE',  ( 280.9755899421581944, 269.7771650631953548, -145.4357337430840289 ) ) ;
#7447 =( GEOMETRIC_REPRESENTATION_CONTEXT ( 3 ) GLOBAL_UNCERTAINTY_ASSIGNED_CONTEXT ( ( #10021 ) ) GLOBAL_UNIT_ASSIGNED_CONTEXT ( ( #21885, #10472, #19475 ) ) REPRESENTATION_CONTEXT ( 'NONE', 'WORKASPACE' ) );
#7448 = EDGE_LOOP ( 'NONE', ( #8208, #22647 ) ) ;
#7449 = FACE_OUTER_BOUND ( 'NONE', #22066, .T. ) ;
#7450 = CARTESIAN_POINT ( 'NONE',  ( 281.4928932188134354, -132.2000000000000455, -177.2000000000013529 ) ) ;
#7451 = CIRCLE ( 'NONE', #20958, 5.249999999999949374 ) ;
#7452 = FACE_OUTER_BOUND ( 'NONE', #20426, .T. ) ;
#7453 = ORIENTED_EDGE ( 'NONE', *, *, #22252, .F. ) ;
#7454 = DIRECTION ( 'NONE',  ( 1.000000000000000000, -3.495664435217746987E-15, -0.000000000000000000 ) ) ;
#7455 = CARTESIAN_POINT ( 'NONE',  ( -5.273354073351990332E-15, -59.79999999999976978, 74.99940828143401461 ) ) ;
#7456 = LINE ( 'NONE', #15207, #21349 ) ;
#7457 = EDGE_LOOP ( 'NONE', ( #2097, #4322, #12967, #20376 ) ) ;
#7458 = CARTESIAN_POINT ( 'NONE',  ( 279.9999999999999432, 272.9999999999999432, -144.9999999999999716 ) ) ;
#7459 = SHAPE_DEFINITION_REPRESENTATION ( #9034, #3124 ) ;
#7460 = CARTESIAN_POINT ( 'NONE',  ( -126.5312127422330519, 89.52572971382308253, -29.19154146838982200 ) ) ;
#7461 = DIRECTION ( 'NONE',  ( 0.000000000000000000, 0.000000000000000000, -1.000000000000000000 ) ) ;
#7462 = DIRECTION ( 'NONE',  ( 0.000000000000000000, 0.4999999999999993339, -0.8660254037844390407 ) ) ;
#7463 = CIRCLE ( 'NONE', #15963, 10.39117206796836079 ) ;
#7464 = VERTEX_POINT ( 'NONE', #20610 ) ;
#7465 = VECTOR ( 'NONE', #7321, 1000.000000000000000 ) ;
#7466 = EDGE_LOOP ( 'NONE', ( #5100, #3745, #4284, #1988 ) ) ;
#7467 = DIRECTION ( 'NONE',  ( 0.000000000000000000, 0.4999999999999993339, -0.8660254037844390407 ) ) ;
#7468 = UNCERTAINTY_MEASURE_WITH_UNIT (LENGTH_MEASURE( 1.000000000000000082E-05 ), #10286, 'distance_accuracy_value', 'NONE');
#7469 = DIRECTION ( 'NONE',  ( 2.775557561562891351E-17, -1.000000000000000000, 0.000000000000000000 ) ) ;
#7470 = CARTESIAN_POINT ( 'NONE',  ( -194.7500000000000568, -494.4690652294800657, 27.50000000000675371 ) ) ;
#7471 = ORIENTED_EDGE ( 'NONE', *, *, #22339, .F. ) ;
#7472 = FACE_OUTER_BOUND ( 'NONE', #17508, .T. ) ;
#7473 = ADVANCED_FACE ( 'NONE', ( #348 ), #17254, .T. ) ;
#7474 = COLOUR_RGB ( '',0.8941176470588234615, 0.8941176470588234615, 0.8941176470588234615 ) ;
#7475 = ORIENTED_EDGE ( 'NONE', *, *, #4358, .F. ) ;
#7476 = AXIS2_PLACEMENT_3D ( 'NONE', #14680, #20444, #22019 ) ;
#7477 = DIRECTION ( 'NONE',  ( 0.000000000000000000, 0.000000000000000000, 1.000000000000000000 ) ) ;
#7478 = DIRECTION ( 'NONE',  ( 0.000000000000000000, 0.000000000000000000, 1.000000000000000000 ) ) ;
#7479 = ORIENTED_EDGE ( 'NONE', *, *, #4688, .T. ) ;
#7480 = VECTOR ( 'NONE', #597, 1000.000000000000000 ) ;
#7481 = DIRECTION ( 'NONE',  ( 0.000000000000000000, -1.000000000000000000, 1.287488025362403787E-15 ) ) ;
#7482 = ADVANCED_FACE ( 'NONE', ( #19163 ), #7830, .F. ) ;
#7483 = CARTESIAN_POINT ( 'NONE',  ( -45.24999999999994316, 100.0000000000000000, 150.2000000000009550 ) ) ;
#7484 = CARTESIAN_POINT ( 'NONE',  ( 1.636246173744687837, -1024.999999999999773, 145.0000119999999697 ) ) ;
#7485 = EDGE_CURVE ( 'NONE', #852, #7964, #9775, .T. ) ;
#7486 = ADVANCED_FACE ( 'NONE', ( #16767 ), #17024, .F. ) ;
#7487 = CARTESIAN_POINT ( 'NONE',  ( 285.1663417894421855, 268.4816199723479713, 146.3683070494395508 ) ) ;
#7488 = CARTESIAN_POINT ( 'NONE',  ( 10.00000000000000178, 9.797174393178825657E-16, -8.000000000000000000 ) ) ;
#7489 = CARTESIAN_POINT ( 'NONE',  ( -7.500000000000000888, -0.7512838658081441023, 1.307818870560639724E-15 ) ) ;
#7490 = ORIENTED_EDGE ( 'NONE', *, *, #23744, .F. ) ;
#7491 = AXIS2_PLACEMENT_3D ( 'NONE', #10324, #8377, #17547 ) ;
#7492 = FACE_OUTER_BOUND ( 'NONE', #1954, .T. ) ;
#7493 = FACE_OUTER_BOUND ( 'NONE', #21611, .T. ) ;
#7494 = EDGE_CURVE ( 'NONE', #18385, #2537, #5894, .T. ) ;
#7496 = ORIENTED_EDGE ( 'NONE', *, *, #12731, .T. ) ;
#7495 = EDGE_LOOP ( 'NONE', ( #18483, #20018, #680, #13342 ) ) ;
#7497 = AXIS2_PLACEMENT_3D ( 'NONE', #12853, #3057, #22082 ) ;
#7498 = CARTESIAN_POINT ( 'NONE',  ( -293.2000000000010118, 30.00000000000087041, -104.9999999999997584 ) ) ;
#7499 = CARTESIAN_POINT ( 'NONE',  ( 5.000000000000000000, 2.342598717236912709, 4.057499999999995666 ) ) ;
#7500 = CARTESIAN_POINT ( 'NONE',  ( 280.2488155364688396, 269.9132285165673011, -145.5679143846942907 ) ) ;
#7501 = VECTOR ( 'NONE', #20752, 1000.000000000000000 ) ;
#7502 = ORIENTED_EDGE ( 'NONE', *, *, #17738, .T. ) ;
#7503 = AXIS2_PLACEMENT_3D ( 'NONE', #17173, #5607, #20785 ) ;
#7504 = CARTESIAN_POINT ( 'NONE',  ( -105.0000000000000000, -29.99999999999998579, 0.000000000000000000 ) ) ;
#7505 = ORIENTED_EDGE ( 'NONE', *, *, #20105, .F. ) ;
#7506 = CARTESIAN_POINT ( 'NONE',  ( 119.6158142514527185, -1087.367367941136308, 32.05500000000640881 ) ) ;
#7507 = VERTEX_POINT ( 'NONE', #19040 ) ;
#7508 = LINE ( 'NONE', #50, #9631 ) ;
#7509 = LINE ( 'NONE', #20431, #22316 ) ;
#7510 = ORIENTED_EDGE ( 'NONE', *, *, #17353, .F. ) ;
#7511 = CIRCLE ( 'NONE', #23714, 2.055000000000001492 ) ;
#7512 = LINE ( 'NONE', #9104, #14509 ) ;
#7513 = VERTEX_POINT ( 'NONE', #13197 ) ;
#7514 = CARTESIAN_POINT ( 'NONE',  ( 23.72540896970402358, -991.9499271393301569, -145.0000000000001421 ) ) ;
#7515 = CARTESIAN_POINT ( 'NONE',  ( -282.2000000000006708, 90.00000000000100897, 32.35000000000001563 ) ) ;
#7516 = AXIS2_PLACEMENT_3D ( 'NONE', #4028, #23407, #6998 ) ;
#7517 = LINE ( 'NONE', #18166, #16518 ) ;
#7518 = ADVANCED_FACE ( 'NONE', ( #18928 ), #22798, .F. ) ;
#7519 = DIRECTION ( 'NONE',  ( 0.000000000000000000, -1.287488025362403787E-15, -1.000000000000000000 ) ) ;
#7520 = CARTESIAN_POINT ( 'NONE',  ( -4.197393957002303999, -7.773935952363655451E-14, -3.503767560748929810 ) ) ;
#7521 = CARTESIAN_POINT ( 'NONE',  ( -281.4928932188135491, -129.2000000000000455, 152.4000000000014268 ) ) ;
#7522 = ADVANCED_FACE ( 'NONE', ( #2624 ), #22545, .T. ) ;
#7523 = EDGE_CURVE ( 'NONE', #16083, #7513, #20990, .T. ) ;
#7524 = ORIENTED_EDGE ( 'NONE', *, *, #9487, .T. ) ;
#7525 = CARTESIAN_POINT ( 'NONE',  ( 119.6158142514525480, -1087.367367941136990, -27.94499999999356632 ) ) ;
#7526 = VECTOR ( 'NONE', #5899, 1000.000000000000000 ) ;
#7527 = CARTESIAN_POINT ( 'NONE',  ( 131.5507733270954134, 81.97201125882388340, -30.65604281379822638 ) ) ;
#7528 = ORIENTED_EDGE ( 'NONE', *, *, #9825, .F. ) ;
#7529 = ADVANCED_FACE ( 'NONE', ( #18674 ), #11319, .T. ) ;
#7530 = CARTESIAN_POINT ( 'NONE',  ( -20.00000000000000000, -1000.000000000000000, -138.9999999999999716 ) ) ;
#7531 = CARTESIAN_POINT ( 'NONE',  ( 0.000000000000000000, 0.000000000000000000, -90.00000000000000000 ) ) ;
#7532 = ADVANCED_FACE ( 'NONE', ( #11853 ), #15103, .F. ) ;
#7533 = CARTESIAN_POINT ( 'NONE',  ( 7.500000000000000000, 2.886751345948125547, -7.198902722707427593 ) ) ;
#7534 = AXIS2_PLACEMENT_3D ( 'NONE', #8879, #3060, #8629 ) ;
#7535 = AXIS2_PLACEMENT_3D ( 'NONE', #16665, #7232, #119 ) ;
#7536 = LINE ( 'NONE', #17206, #1010 ) ;
#7537 = DIRECTION ( 'NONE',  ( 1.000000000000000000, 0.000000000000000000, 0.000000000000000000 ) ) ;
#7538 = ITEM_DEFINED_TRANSFORMATION ( 'NONE', 'NONE', #15442,  #11210 ) ;
#7539 = ORIENTED_EDGE ( 'NONE', *, *, #16139, .T. ) ;
#7540 = CYLINDRICAL_SURFACE ( 'NONE', #5199, 2.649999999999999467 ) ;
#7541 = EDGE_LOOP ( 'NONE', ( #7815, #2364, #10458, #22414 ) ) ;
#7542 = DIRECTION ( 'NONE',  ( 0.000000000000000000, 0.7071067811865485719, 0.7071067811865465735 ) ) ;
#7543 = CARTESIAN_POINT ( 'NONE',  ( 1.500000000000001332, 0.000000000000000000, 0.000000000000000000 ) ) ;
#7544 = B_SPLINE_CURVE_WITH_KNOTS ( 'NONE', 3,
 ( #21254, #15944, #4705, #12115, #23284, #20138 ),
 .UNSPECIFIED., .F., .F.,
 ( 4, 2, 4 ),
 ( 0.000000000000000000, 0.002307655110370376069, 0.004615310220740751271 ),
 .UNSPECIFIED. ) ;
#7545 = VECTOR ( 'NONE', #19872, 1000.000000000000000 ) ;
#7546 = LINE ( 'NONE', #14934, #4422 ) ;
#7547 = VERTEX_POINT ( 'NONE', #4197 ) ;
#7548 = CARTESIAN_POINT ( 'NONE',  ( 7.497491405671719455, 144.8060344827586334, -2.775557561562891351E-14 ) ) ;
#7549 = DIRECTION ( 'NONE',  ( -1.000000000000000000, -0.000000000000000000, -0.000000000000000000 ) ) ;
#7550 = AXIS2_PLACEMENT_3D ( 'NONE', #12962, #3723, #20387 ) ;
#7551 = FACE_OUTER_BOUND ( 'NONE', #11244, .T. ) ;
#7552 = CARTESIAN_POINT ( 'NONE',  ( -7.500000000000000000, -4.330127018922198090, -7.422398894150034288 ) ) ;
#7553 = FACE_OUTER_BOUND ( 'NONE', #6008, .T. ) ;
#7554 = DIRECTION ( 'NONE',  ( 0.000000000000000000, 0.4999999999999990008, -0.8660254037844391517 ) ) ;
#7555 = CARTESIAN_POINT ( 'NONE',  ( -107.6499999999999915, 30.00000000000001421, 3.000000000000001332 ) ) ;
#7556 = AXIS2_PLACEMENT_3D ( 'NONE', #6063, #9826, #17305 ) ;
#7557 = VERTEX_POINT ( 'NONE', #22431 ) ;
#7558 = ADVANCED_BREP_SHAPE_REPRESENTATION ( '', ( #20059, #11210 ), #3838 ) ;
#7559 = CARTESIAN_POINT ( 'NONE',  ( 5.000000000000000000, 2.342598717236902939, -4.057500000000001883 ) ) ;
#7560 = CARTESIAN_POINT ( 'NONE',  ( -146.0000000000000853, -204.4690652294807478, 30.00000000000641620 ) ) ;
#7561 = ORIENTED_EDGE ( 'NONE', *, *, #13717, .F. ) ;
#7562 = CARTESIAN_POINT ( 'NONE',  ( 8.964804008826853021, 4.586179404162092688, 200.0000119999999413 ) ) ;
#7563 = CARTESIAN_POINT ( 'NONE',  ( 145.0000000000000284, -500.0000000000000000, 32.50000000000001421 ) ) ;
#7564 = EDGE_CURVE ( 'NONE', #1816, #7788, #13651, .T. ) ;
#7565 = ADVANCED_FACE ( 'NONE', ( #5792 ), #2391, .F. ) ;
#7566 = AXIS2_PLACEMENT_3D ( 'NONE', #18523, #18060, #11073 ) ;
#7567 = EDGE_CURVE ( 'NONE', #12111, #539, #5090, .T. ) ;
#7568 = CARTESIAN_POINT ( 'NONE',  ( -9.999999999999998224, -6.123233995736763324E-16, 200.0000060000000133 ) ) ;
#7569 = ORIENTED_EDGE ( 'NONE', *, *, #2025, .F. ) ;
#7570 = CARTESIAN_POINT ( 'NONE',  ( 1.983456134378398743E-14, -52.79999999999986215, 1.831306136874101694E-13 ) ) ;
#7571 = CARTESIAN_POINT ( 'NONE',  ( 1.819057724962738742E-14, -56.79999999999984794, 1.970645868709647811E-13 ) ) ;
#7572 = CARTESIAN_POINT ( 'NONE',  ( 8.737863883542583920, -5.036189803708986723, 200.0000119999999981 ) ) ;
#7573 = VERTEX_POINT ( 'NONE', #6488 ) ;
#7574 = DIRECTION ( 'NONE',  ( 1.000000000000000000, 0.000000000000000000, 0.000000000000000000 ) ) ;
#7575 = CARTESIAN_POINT ( 'NONE',  ( -136.8330323738929621, -1072.812977866783285, 31.25900233431395137 ) ) ;
#7576 = CARTESIAN_POINT ( 'NONE',  ( 119.6158142514525764, -1087.367367941136990, -32.05499999999356930 ) ) ;
#7577 = ORIENTED_EDGE ( 'NONE', *, *, #3147, .F. ) ;
#7578 = CARTESIAN_POINT ( 'NONE',  ( 282.6188186979285888, 272.3436892194421262, -145.4976310729377644 ) ) ;
#7579 = PRODUCT_CONTEXT ( 'NONE', #16775, 'mechanical' ) ;
#7580 = DIRECTION ( 'NONE',  ( 0.000000000000000000, 0.000000000000000000, 1.000000000000000000 ) ) ;
#7581 = CARTESIAN_POINT ( 'NONE',  ( 21.68333333333335844, -89.99999999999998579, 0.000000000000000000 ) ) ;
#7582 = DIRECTION ( 'NONE',  ( -0.000000000000000000, -0.000000000000000000, 1.000000000000000000 ) ) ;
#7583 = CARTESIAN_POINT ( 'NONE',  ( -175.1609685624542578, -1088.719770019218458, -29.99999999999322498 ) ) ;
#7584 = ORIENTED_EDGE ( 'NONE', *, *, #23025, .F. ) ;
#7585 = ORIENTED_EDGE ( 'NONE', *, *, #23704, .F. ) ;
#7586 = CARTESIAN_POINT ( 'NONE',  ( -24.99999999999999645, -2.129009867111508370E-15, 145.0000059999999849 ) ) ;
#7587 = DIRECTION ( 'NONE',  ( -1.110223024625157172E-14, 0.000000000000000000, -1.000000000000000000 ) ) ;
#7588 = ADVANCED_FACE ( 'NONE', ( #6733 ), #15925, .F. ) ;
#7589 = PRODUCT_DEFINITION_CONTEXT ( 'detailed design', #14786, 'design' ) ;
#7590 = AXIS2_PLACEMENT_3D ( 'NONE', #5926, #10163, #4101 ) ;
#7591 = CARTESIAN_POINT ( 'NONE',  ( -7.500000000000000000, -4.330127018922199866, -1.000000000000000888 ) ) ;
#7592 = EDGE_CURVE ( 'NONE', #14316, #2992, #7044, .T. ) ;
#7593 = CARTESIAN_POINT ( 'NONE',  ( 25.00000000000000000, 4.926831259382130415E-15, 145.0000119999999697 ) ) ;
#7594 = EDGE_LOOP ( 'NONE', ( #19713, #22218, #18798, #13305 ) ) ;
#7595 = AXIS2_PLACEMENT_3D ( 'NONE', #23278, #1552, #21713 ) ;
#7596 = CARTESIAN_POINT ( 'NONE',  ( -285.2000000000010687, -19.99999999999898392, 105.0000000000000000 ) ) ;
#7597 = ORIENTED_EDGE ( 'NONE', *, *, #10081, .F. ) ;
#7598 = B_SPLINE_CURVE_WITH_KNOTS ( 'NONE', 3,
 ( #21920, #5866, #20473, #16632, #3921, #14825 ),
 .UNSPECIFIED., .F., .F.,
 ( 4, 2, 4 ),
 ( 0.003358874760055550156, 0.004541967308452096383, 0.005725059856848641743 ),
 .UNSPECIFIED. ) ;
#7599 = CARTESIAN_POINT ( 'NONE',  ( 158.0000000000000284, -500.0000000000000000, -32.64999999999995595 ) ) ;
#7600 = DIRECTION ( 'NONE',  ( -0.9423651898111408132, -0.3345860861306287348, 6.982962677686266711E-15 ) ) ;
#7601 = ORIENTED_EDGE ( 'NONE', *, *, #12482, .F. ) ;
#7602 = CARTESIAN_POINT ( 'NONE',  ( -3.280815508853482498, -7.221948645665452915, -7.591546097228404122 ) ) ;
#7603 = CARTESIAN_POINT ( 'NONE',  ( 285.1999999999999318, 269.9999999999999432, 146.4928932188134638 ) ) ;
#7604 = CARTESIAN_POINT ( 'NONE',  ( 11.07878015919984982, -1022.470824010819570, 145.0000119999999697 ) ) ;
#7605 = AXIS2_PLACEMENT_3D ( 'NONE', #8929, #7441, #21704 ) ;
#7606 = CARTESIAN_POINT ( 'NONE',  ( 285.0335297745771186, 269.1488036478618824, 146.2439791848364621 ) ) ;
#7607 = DIRECTION ( 'NONE',  ( -0.000000000000000000, -0.000000000000000000, 1.000000000000000000 ) ) ;
#7608 = DIRECTION ( 'NONE',  ( 1.000000000000000000, 0.000000000000000000, -0.000000000000000000 ) ) ;
#7609 = ORIENTED_EDGE ( 'NONE', *, *, #14111, .F. ) ;
#7610 = CARTESIAN_POINT ( 'NONE',  ( 0.000000000000000000, 0.000000000000000000, -4.974599999999998801 ) ) ;
#7611 = DIRECTION ( 'NONE',  ( -1.000000000000000000, 1.408839003528726857E-14, 6.982962677686266711E-15 ) ) ;
#7612 = AXIS2_PLACEMENT_3D ( 'NONE', #22063, #9046, #7212 ) ;
#7613 = ADVANCED_FACE ( 'NONE', ( #13782 ), #10152, .T. ) ;
#7614 = CIRCLE ( 'NONE', #15736, 20.00000000000000000 ) ;
#7616 = EDGE_LOOP ( 'NONE', ( #20, #14324, #19764, #5532 ) ) ;
#7615 = VERTEX_POINT ( 'NONE', #10379 ) ;
#7617 = EDGE_CURVE ( 'NONE', #711, #20235, #23156, .T. ) ;
#7618 = DIRECTION ( 'NONE',  ( 0.000000000000000000, 1.224646799147353207E-16, 1.000000000000000000 ) ) ;
#7619 = CARTESIAN_POINT ( 'NONE',  ( 0.000000000000000000, 0.000000000000000000, -125.0000000000000000 ) ) ;
#7620 = VERTEX_POINT ( 'NONE', #14129 ) ;
#7621 = CARTESIAN_POINT ( 'NONE',  ( -135.0351526491285199, -1076.095746396249979, 32.00444854364506853 ) ) ;
#7622 = ORIENTED_EDGE ( 'NONE', *, *, #5227, .T. ) ;
#7623 = EDGE_CURVE ( 'NONE', #3666, #15218, #2435, .T. ) ;
#7624 = CARTESIAN_POINT ( 'NONE',  ( 284.9324007871372828, 269.4810649015076933, -146.1807969192697385 ) ) ;
#7625 = ORIENTED_EDGE ( 'NONE', *, *, #14939, .T. ) ;
#7626 = LINE ( 'NONE', #22111, #6913 ) ;
#7627 = FACE_OUTER_BOUND ( 'NONE', #1553, .T. ) ;
#7628 = EDGE_CURVE ( 'NONE', #19884, #14233, #9411, .T. ) ;
#7629 = AXIS2_PLACEMENT_3D ( 'NONE', #11330, #2106, #9498 ) ;
#7630 = CONTEXT_DEPENDENT_SHAPE_REPRESENTATION ( #4482, #13965 ) ;
#7631 = ORIENTED_EDGE ( 'NONE', *, *, #15873, .F. ) ;
#7632 = AXIS2_PLACEMENT_3D ( 'NONE', #14719, #4177, #329 ) ;
#7633 = CARTESIAN_POINT ( 'NONE',  ( 125.2216071840750402, -1091.349008980711915, 32.18904844917292252 ) ) ;
#7634 = VERTEX_POINT ( 'NONE', #10140 ) ;
#7635 = CARTESIAN_POINT ( 'NONE',  ( -129.0269476471448513, 85.88978664864519885, 31.53271418707683083 ) ) ;
#7636 = PRESENTATION_STYLE_ASSIGNMENT (( #280 ) ) ;
#7637 = DIRECTION ( 'NONE',  ( -0.000000000000000000, -0.000000000000000000, 1.000000000000000000 ) ) ;
#7638 = CARTESIAN_POINT ( 'NONE',  ( 0.000000000000000000, -1000.000000000000000, -125.0000000000001137 ) ) ;
#7639 = ORIENTED_EDGE ( 'NONE', *, *, #22167, .F. ) ;
#7640 = CARTESIAN_POINT ( 'NONE',  ( 0.000000000000000000, 0.000000000000000000, 90.00000000000000000 ) ) ;
#7641 = DIRECTION ( 'NONE',  ( 0.000000000000000000, 0.000000000000000000, -1.000000000000000000 ) ) ;
#7642 = ORIENTED_EDGE ( 'NONE', *, *, #14172, .F. ) ;
#7643 = VECTOR ( 'NONE', #12564, 1000.000000000000000 ) ;
#7644 = CIRCLE ( 'NONE', #9593, 7.499999999999996447 ) ;
#7645 = CARTESIAN_POINT ( 'NONE',  ( -285.2000000000014666, -127.0000000000000568, -146.4928932188134070 ) ) ;
#7646 = CARTESIAN_POINT ( 'NONE',  ( 131.6954086522101193, 81.73939080771404520, -28.73951976925631868 ) ) ;
#7647 = VECTOR ( 'NONE', #5244, 1000.000000000000000 ) ;
#7648 = CIRCLE ( 'NONE', #14618, 45.00000000000000711 ) ;
#7649 = DIRECTION ( 'NONE',  ( 0.000000000000000000, 1.000000000000000000, -0.000000000000000000 ) ) ;
#7650 = EDGE_CURVE ( 'NONE', #13664, #10493, #16040, .T. ) ;
#7651 = CARTESIAN_POINT ( 'NONE',  ( -281.3689414351990763, 272.8938770989752811, -145.2488155364688396 ) ) ;
#7652 = EDGE_CURVE ( 'NONE', #14389, #14374, #21717, .T. ) ;
#7653 = B_SPLINE_CURVE_WITH_KNOTS ( 'NONE', 3,
 ( #483, #7842, #15224, #20507, #16899, #365, #13573, #17141, #19051, #4812, #21355, #17607, #17493, #23167, #598, #20886, #6631, #10268, #14027, #22681, #6151, #6503, #6274, #8321, #23031, #13682, #11745, #7961, #15343, #19406, #22914, #941 ),
 .UNSPECIFIED., .F., .F.,
 ( 4, 2, 2, 2, 2, 2, 2, 2, 2, 2, 2, 2, 2, 2, 2, 4 ),
 ( 0.000000000000000000, 0.0004914281572963851439, 0.0009828563145927702877, 0.001474284471889155540, 0.001965712629185540575, 0.002457140786481926045, 0.002948568943778311080, 0.003931425258371084620, 0.004422853415667466620, 0.004914281572963847752, 0.005405709730260229752, 0.005897137887556611752, 0.006388566044852992884, 0.006879994202149374016, 0.007371422359445756016, 0.007862850516742138016 ),
 .UNSPECIFIED. ) ;
#7654 = VECTOR ( 'NONE', #19873, 1000.000000000000000 ) ;
#7655 = FACE_OUTER_BOUND ( 'NONE', #5868, .T. ) ;
#7656 = CARTESIAN_POINT ( 'NONE',  ( 123.3268328482426881, -1093.890927824661276, 31.65640384616908420 ) ) ;
#7657 = ADVANCED_FACE ( 'NONE', ( #6849 ), #8310, .F. ) ;
#7658 = EDGE_LOOP ( 'NONE', ( #21127, #22080, #14017, #17202 ) ) ;
#7659 = CARTESIAN_POINT ( 'NONE',  ( 8.055391459054620285, -976.2768473852548823, 145.0000119999999981 ) ) ;
#7660 = EDGE_CURVE ( 'NONE', #22176, #19928, #23254, .T. ) ;
#7661 = ORIENTED_EDGE ( 'NONE', *, *, #21593, .T. ) ;
#7663 = CARTESIAN_POINT ( 'NONE',  ( -100.0000000000000000, 249.9999999999999716, 125.0000000000000284 ) ) ;
#7662 = AXIS2_PLACEMENT_3D ( 'NONE', #4160, #308, #443 ) ;
#7664 = CARTESIAN_POINT ( 'NONE',  ( 5.000000000000000000, -2.342598717236900718, 4.057500000000001883 ) ) ;
#7666 = VECTOR ( 'NONE', #5627, 1000.000000000000000 ) ;
#7665 =( GEOMETRIC_REPRESENTATION_CONTEXT ( 3 ) GLOBAL_UNCERTAINTY_ASSIGNED_CONTEXT ( ( #22193 ) ) GLOBAL_UNIT_ASSIGNED_CONTEXT ( ( #4714, #6880, #19797 ) ) REPRESENTATION_CONTEXT ( 'NONE', 'WORKASPACE' ) );
#7667 = AXIS2_PLACEMENT_3D ( 'NONE', #6742, #22705, #13592 ) ;
#7668 = CARTESIAN_POINT ( 'NONE',  ( -5.000000000000000888, 6.123233995736767268E-16, -25.03750572909317285 ) ) ;
#7669 = AXIS2_PLACEMENT_3D ( 'NONE', #8666, #17959, #2969 ) ;
#7670 = ORIENTED_EDGE ( 'NONE', *, *, #14092, .F. ) ;
#7671 = DIRECTION ( 'NONE',  ( -0.000000000000000000, -0.000000000000000000, 1.000000000000000000 ) ) ;
#7672 = AXIS2_PLACEMENT_3D ( 'NONE', #7998, #634, #18968 ) ;
#7673 = AXIS2_PLACEMENT_3D ( 'NONE', #17282, #726, #10057 ) ;
#7674 = DIRECTION ( 'NONE',  ( 0.000000000000000000, 0.000000000000000000, 1.000000000000000000 ) ) ;
#7675 = CARTESIAN_POINT ( 'NONE',  ( 37.61698748598424658, 140.0355749532214986, -2.775557561562891351E-14 ) ) ;
#7676 = CYLINDRICAL_SURFACE ( 'NONE', #8254, 2.500000000000002220 ) ;
#7677 = DIRECTION ( 'NONE',  ( -1.000000000000000000, 0.000000000000000000, 0.000000000000000000 ) ) ;
#7678 = DIRECTION ( 'NONE',  ( -0.000000000000000000, 0.000000000000000000, 1.000000000000000000 ) ) ;
#7679 = AXIS2_PLACEMENT_3D ( 'NONE', #14075, #19345, #15745 ) ;
#7680 = CARTESIAN_POINT ( 'NONE',  ( -7.908228835406498902, 3.123118350879302341, -7.776694659841278501 ) ) ;
#7681 = EDGE_LOOP ( 'NONE', ( #22011, #10510, #13041, #17510 ) ) ;
#7682 = CYLINDRICAL_SURFACE ( 'NONE', #14982, 2.649999999999985700 ) ;
#7683 = CARTESIAN_POINT ( 'NONE',  ( -45.00000000000000000, 250.0000000000000000, 0.000000000000000000 ) ) ;
#7684 = EDGE_LOOP ( 'NONE', ( #17817, #1233, #2896, #8593 ) ) ;
#7685 = ORIENTED_EDGE ( 'NONE', *, *, #20929, .T. ) ;
#7686 = MECHANICAL_DESIGN_GEOMETRIC_PRESENTATION_REPRESENTATION (  '', ( #3437 ), #8855 ) ;
#7687 = FACE_OUTER_BOUND ( 'NONE', #17602, .T. ) ;
#7688 = DIRECTION ( 'NONE',  ( 0.000000000000000000, -2.838638415234739015E-14, -1.000000000000000000 ) ) ;
#7689 = AXIS2_PLACEMENT_3D ( 'NONE', #10575, #8746, #16111 ) ;
#7691 = AXIS2_PLACEMENT_3D ( 'NONE', #23677, #18018, #7138 ) ;
#7690 =( GEOMETRIC_REPRESENTATION_CONTEXT ( 3 ) GLOBAL_UNCERTAINTY_ASSIGNED_CONTEXT ( ( #16664 ) ) GLOBAL_UNIT_ASSIGNED_CONTEXT ( ( #20960, #6238, #15662 ) ) REPRESENTATION_CONTEXT ( 'NONE', 'WORKASPACE' ) );
#7692 = CIRCLE ( 'NONE', #11571, 2.499999999999946709 ) ;
#7693 = VECTOR ( 'NONE', #7289, 1000.000000000000000 ) ;
#7694 = CARTESIAN_POINT ( 'NONE',  ( 2.500000000000002220, 2.500728763858895382E-16, -2.041999999999999815 ) ) ;
#7695 = AXIS2_PLACEMENT_3D ( 'NONE', #18397, #186, #7537 ) ;
#7696 = AXIS2_PLACEMENT_3D ( 'NONE', #21705, #14831, #1756 ) ;
#7697 = VERTEX_POINT ( 'NONE', #21591 ) ;
#7698 = EDGE_CURVE ( 'NONE', #9956, #11870, #15957, .T. ) ;
#7699 = CARTESIAN_POINT ( 'NONE',  ( 0.000000000000000000, 2.357898499370433054, -1.951563910473907981E-15 ) ) ;
#7700 = CARTESIAN_POINT ( 'NONE',  ( 2.500000000000002220, 1.178949249685218970, 2.041999999999998483 ) ) ;
#7701 = EDGE_CURVE ( 'NONE', #8456, #6907, #11741, .T. ) ;
#7702 = CARTESIAN_POINT ( 'NONE',  ( 1.308996938995748094, -9.999999999999992895, 200.0000120000000265 ) ) ;
#7703 = EDGE_CURVE ( 'NONE', #14948, #22288, #20118, .T. ) ;
#7704 = ORIENTED_EDGE ( 'NONE', *, *, #22227, .F. ) ;
#7705 = DIRECTION ( 'NONE',  ( 0.000000000000000000, 0.000000000000000000, 1.000000000000000000 ) ) ;
#7706 = LINE ( 'NONE', #2130, #9298 ) ;
#7707 = EDGE_CURVE ( 'NONE', #3284, #15717, #21811, .T. ) ;
#7708 = CARTESIAN_POINT ( 'NONE',  ( 0.000000000000000000, 0.000000000000000000, -90.00000000000000000 ) ) ;
#7709 = ORIENTED_EDGE ( 'NONE', *, *, #23183, .F. ) ;
#7710 = DIRECTION ( 'NONE',  ( 0.000000000000000000, 0.000000000000000000, -1.000000000000000000 ) ) ;
#7711 = APPLICATION_PROTOCOL_DEFINITION ( 'draft international standard', 'automotive_design', 1998, #13123 ) ;
#7712 = LINE ( 'NONE', #22542, #8515 ) ;
#7713 = EDGE_CURVE ( 'NONE', #21635, #10663, #16284, .T. ) ;
#7715 = VECTOR ( 'NONE', #19064, 1000.000000000000114 ) ;
#7714 = AXIS2_PLACEMENT_3D ( 'NONE', #20448, #1725, #5717 ) ;
#7716 = EDGE_CURVE ( 'NONE', #20294, #13434, #3211, .T. ) ;
#7718 = CARTESIAN_POINT ( 'NONE',  ( -20.00000000000000000, 2.449293598294706513E-15, 124.9999999999999716 ) ) ;
#7717 = COLOUR_RGB ( '',0.8941176470588234615, 0.8941176470588234615, 0.8941176470588234615 ) ;
#7719 = CARTESIAN_POINT ( 'NONE',  ( 90.00000000000000000, 2.914335439641035919E-13, 129.9038105676659711 ) ) ;
#7720 = VECTOR ( 'NONE', #9919, 1000.000000000000000 ) ;
#7721 = AXIS2_PLACEMENT_3D ( 'NONE', #17394, #22025, #11549 ) ;
#7722 = ORIENTED_EDGE ( 'NONE', *, *, #22406, .T. ) ;
#7723 = EDGE_LOOP ( 'NONE', ( #15081, #18971, #8325, #22334 ) ) ;
#7724 = LINE ( 'NONE', #22434, #20315 ) ;
#7725 = CARTESIAN_POINT ( 'NONE',  ( -281.4928932188134354, -127.0000000000000568, -152.4000000000012847 ) ) ;
#7726 = AXIS2_PLACEMENT_3D ( 'NONE', #5266, #8738, #19456 ) ;
#7727 = EDGE_LOOP ( 'NONE', ( #12026, #11175 ) ) ;
#7728 = DIRECTION ( 'NONE',  ( -1.000000000000000000, 0.000000000000000000, 0.000000000000000000 ) ) ;
#7729 = ADVANCED_FACE ( 'NONE', ( #18413, #1751 ), #5275, .T. ) ;
#7730 = CARTESIAN_POINT ( 'NONE',  ( 2.500000000000002220, 0.000000000000000000, 2.041999999999999815 ) ) ;
#7731 = AXIS2_PLACEMENT_3D ( 'NONE', #9446, #5572, #23798 ) ;
#7732 = ORIENTED_EDGE ( 'NONE', *, *, #9789, .T. ) ;
#7733 = LINE ( 'NONE', #6276, #15284 ) ;
#7734 = VECTOR ( 'NONE', #13179, 1000.000000000000000 ) ;
#7735 = AXIS2_PLACEMENT_3D ( 'NONE', #2017, #20607, #14972 ) ;
#7736 = AXIS2_PLACEMENT_3D ( 'NONE', #17820, #2832, #23238 ) ;
#7737 = ORIENTED_EDGE ( 'NONE', *, *, #7617, .T. ) ;
#7738 = DIRECTION ( 'NONE',  ( 0.000000000000000000, -1.287488025362403787E-15, -1.000000000000000000 ) ) ;
#7739 = ORIENTED_EDGE ( 'NONE', *, *, #22085, .F. ) ;
#7740 = ORIENTED_EDGE ( 'NONE', *, *, #7398, .F. ) ;
#7741 = DIRECTION ( 'NONE',  ( -1.000000000000000000, -0.000000000000000000, -0.000000000000000000 ) ) ;
#7742 = CARTESIAN_POINT ( 'NONE',  ( -31.74999999999995737, 5.204748896376250699E-16, -4.250000000000000000 ) ) ;
#7743 = EDGE_CURVE ( 'NONE', #11281, #23782, #1873, .T. ) ;
#7744 = CARTESIAN_POINT ( 'NONE',  ( -8.050035159177529209, -1023.725317947569579, -145.0000000000001421 ) ) ;
#7745 = EDGE_CURVE ( 'NONE', #19747, #13550, #9026, .T. ) ;
#7746 = CARTESIAN_POINT ( 'NONE',  ( -280.0000000000000000, 270.0000000000000000, -144.9999999999999716 ) ) ;
#7747 = CARTESIAN_POINT ( 'NONE',  ( 0.000000000000000000, -1.178949249685213863, 2.042000000000001148 ) ) ;
#7748 = CARTESIAN_POINT ( 'NONE',  ( 0.000000000000000000, 0.000000000000000000, -10.00000000000000000 ) ) ;
#7749 = CARTESIAN_POINT ( 'NONE',  ( 155.0000000000000284, -500.0000000000000000, 30.00000000000001421 ) ) ;
#7750 = ORIENTED_EDGE ( 'NONE', *, *, #13281, .F. ) ;
#7751 = CARTESIAN_POINT ( 'NONE',  ( -146.0000000000005116, -494.4690652294800657, -29.99999999999356604 ) ) ;
#7752 = FACE_BOUND ( 'NONE', #13351, .T. ) ;
#7753 = CARTESIAN_POINT ( 'NONE',  ( -0.3875187462251565851, -8.436519985395204202, -7.781689322724289148 ) ) ;
#7754 = SURFACE_STYLE_USAGE ( .BOTH. , #621 ) ;
#7756 = ORIENTED_EDGE ( 'NONE', *, *, #19801, .T. ) ;
#7755 = ORIENTED_EDGE ( 'NONE', *, *, #21249, .T. ) ;
#7757 = CARTESIAN_POINT ( 'NONE',  ( -136.8705256357208668, -1072.742444906768242, -28.88783501520649821 ) ) ;
#7758 = CARTESIAN_POINT ( 'NONE',  ( 280.6220388411722411, 271.9582675804705900, -148.1956429438695011 ) ) ;
#7759 = ORIENTED_EDGE ( 'NONE', *, *, #19963, .F. ) ;
#7760 = CARTESIAN_POINT ( 'NONE',  ( -135.7895026000614678, -1074.740959209980247, 27.50000000000646239 ) ) ;
#7761 = ORIENTED_EDGE ( 'NONE', *, *, #20262, .T. ) ;
#7762 = CARTESIAN_POINT ( 'NONE',  ( 0.000000000000000000, 0.000000000000000000, -10.00000000000000000 ) ) ;
#7763 = ORIENTED_EDGE ( 'NONE', *, *, #12402, .F. ) ;
#7764 = DIRECTION ( 'NONE',  ( -0.000000000000000000, -0.000000000000000000, -1.000000000000000000 ) ) ;
#7765 = CARTESIAN_POINT ( 'NONE',  ( -44.99999999999997868, -59.79999999999936477, 195.0000000000001990 ) ) ;
#7766 = ITEM_DEFINED_TRANSFORMATION ( 'NONE', 'NONE', #20436,  #11210 ) ;
#7767 = ORIENTED_EDGE ( 'NONE', *, *, #17835, .F. ) ;
#7768 = CARTESIAN_POINT ( 'NONE',  ( -100.0000000000000000, 0.000000000000000000, 0.000000000000000000 ) ) ;
#7769 = ORIENTED_EDGE ( 'NONE', *, *, #18990, .F. ) ;
#7770 = CARTESIAN_POINT ( 'NONE',  ( 22.46856765586026583, -988.9159012424156572, -145.0000000000001421 ) ) ;
#7771 = CARTESIAN_POINT ( 'NONE',  ( 0.000000000000000000, -2.342598717236900718, 4.057500000000001883 ) ) ;
#7772 = CARTESIAN_POINT ( 'NONE',  ( -285.2000000000012960, -74.99999999999899103, 90.00000000000000000 ) ) ;
#7773 = VERTEX_POINT ( 'NONE', #13040 ) ;
#7774 = CARTESIAN_POINT ( 'NONE',  ( -281.4928932188134354, 267.7999999999999545, -147.1999999999999318 ) ) ;
#7775 = EDGE_LOOP ( 'NONE', ( #13596, #19613 ) ) ;
#7776 = SURFACE_SIDE_STYLE ('',( #10951 ) ) ;
#7777 = DIRECTION ( 'NONE',  ( -0.000000000000000000, -0.000000000000000000, 1.000000000000000000 ) ) ;
#7778 = DIRECTION ( 'NONE',  ( -0.000000000000000000, -0.000000000000000000, -1.000000000000000000 ) ) ;
#7779 = CARTESIAN_POINT ( 'NONE',  ( 280.6847249064868492, 273.0299999999999159, 145.1244295015775947 ) ) ;
#7780 = DIRECTION ( 'NONE',  ( 1.000000000000000000, 0.000000000000000000, 0.000000000000000000 ) ) ;
#7781 = ORIENTED_EDGE ( 'NONE', *, *, #10570, .T. ) ;
#7782 = PRODUCT_DEFINITION_SHAPE ( 'NONE', 'NONE',  #23886 ) ;
#7783 = CARTESIAN_POINT ( 'NONE',  ( 146.4450000000001921, -210.0000000000003411, -27.49999999999356604 ) ) ;
#7784 = DIRECTION ( 'NONE',  ( 0.000000000000000000, -1.177509268541832635E-16, 1.000000000000000000 ) ) ;
#7785 = CARTESIAN_POINT ( 'NONE',  ( 123.4701789281961766, -1093.702342252439848, 31.88926668738014669 ) ) ;
#7786 = VERTEX_POINT ( 'NONE', #3679 ) ;
#7787 = CARTESIAN_POINT ( 'NONE',  ( 2.500000000000000000, 2.357898499370431722, -2.818925648462311528E-15 ) ) ;
#7788 = VERTEX_POINT ( 'NONE', #9128 ) ;
#7789 = FACE_BOUND ( 'NONE', #7117, .T. ) ;
#7790 = CARTESIAN_POINT ( 'NONE',  ( 2.500000000000000888, 3.061616997868384127E-16, -4.974599999999998801 ) ) ;
#7791 = ORIENTED_EDGE ( 'NONE', *, *, #863, .F. ) ;
#7792 = CYLINDRICAL_SURFACE ( 'NONE', #22138, 19.99999999999999289 ) ;
#7793 = ORIENTED_EDGE ( 'NONE', *, *, #17108, .T. ) ;
#7794 = CARTESIAN_POINT ( 'NONE',  ( 32.35000000000001563, 90.00000000000000000, 3.000000000000000000 ) ) ;
#7795 = PLANE ( 'NONE',  #13076 ) ;
#7796 = EDGE_CURVE ( 'NONE', #14436, #3630, #881, .T. ) ;
#7797 = DIRECTION ( 'NONE',  ( 1.000000000000000000, 0.000000000000000000, 0.000000000000000000 ) ) ;
#7798 = CYLINDRICAL_SURFACE ( 'NONE', #13306, 2.500000000000002220 ) ;
#7799 = CARTESIAN_POINT ( 'NONE',  ( 281.4928932188133217, -127.0000000000000568, 152.4000000000014268 ) ) ;
#7800 = EDGE_CURVE ( 'NONE', #1487, #17506, #7186, .T. ) ;
#7801 = FACE_OUTER_BOUND ( 'NONE', #1173, .T. ) ;
#7802 = EDGE_CURVE ( 'NONE', #3444, #2834, #14045, .T. ) ;
#7803 = CARTESIAN_POINT ( 'NONE',  ( -7.500000000000000000, -3.948305025207388130, -7.349903712356284480 ) ) ;
#7804 = ORIENTED_EDGE ( 'NONE', *, *, #17971, .T. ) ;
#7805 = FILL_AREA_STYLE ('',( #9632 ) ) ;
#7806 = CARTESIAN_POINT ( 'NONE',  ( 70.00000000000000000, -112.6666666666666714, 3.000000000000001332 ) ) ;
#7807 = DIRECTION ( 'NONE',  ( 1.000000000000000000, 0.000000000000000000, 0.000000000000000000 ) ) ;
#7808 = ADVANCED_FACE ( 'NONE', ( #6235 ), #3954, .F. ) ;
#7809 = EDGE_LOOP ( 'NONE', ( #19533, #17662, #23628, #13671 ) ) ;
#7810 = AXIS2_PLACEMENT_3D ( 'NONE', #1320, #13808, #8700 ) ;
#7811 = ORIENTED_EDGE ( 'NONE', *, *, #16241, .F. ) ;
#7812 = DIRECTION ( 'NONE',  ( 0.000000000000000000, 0.000000000000000000, -1.000000000000000000 ) ) ;
#7813 = CYLINDRICAL_SURFACE ( 'NONE', #8051, 7.500000000000000000 ) ;
#7814 = FACE_OUTER_BOUND ( 'NONE', #8230, .T. ) ;
#7815 = ORIENTED_EDGE ( 'NONE', *, *, #460, .F. ) ;
#7816 = DIRECTION ( 'NONE',  ( 0.000000000000000000, 0.000000000000000000, 1.000000000000000000 ) ) ;
#7817 = DIRECTION ( 'NONE',  ( -0.000000000000000000, -0.000000000000000000, 1.000000000000000000 ) ) ;
#7818 = DIRECTION ( 'NONE',  ( 1.000000000000000000, -0.000000000000000000, 6.982962677686266711E-15 ) ) ;
#7819 = EDGE_LOOP ( 'NONE', ( #21601, #18591, #7524, #4617 ) ) ;
#7820 = CARTESIAN_POINT ( 'NONE',  ( -91.18044947428874991, -112.7436279071535097, -2.775557561562891351E-14 ) ) ;
#7821 = B_SPLINE_CURVE_WITH_KNOTS ( 'NONE', 3,
 ( #12945, #3833, #14850, #18441, #10895, #18327 ),
 .UNSPECIFIED., .F., .F.,
 ( 4, 2, 4 ),
 ( 0.000000000000000000, 0.002307655110370371299, 0.004615310220740742597 ),
 .UNSPECIFIED. ) ;
#7822 = CARTESIAN_POINT ( 'NONE',  ( 2.500000000000000000, 2.357898499370432166, -2.385244779468109755E-15 ) ) ;
#7823 = DIRECTION ( 'NONE',  ( -1.000000000000000000, -0.000000000000000000, -0.000000000000000000 ) ) ;
#7824 = VERTEX_POINT ( 'NONE', #4169 ) ;
#7825 = CARTESIAN_POINT ( 'NONE',  ( 281.7350371479512319, 269.1333820183295416, -145.8708543776411091 ) ) ;
#7826 = CIRCLE ( 'NONE', #20933, 2.055000000000000160 ) ;
#7827 = SHAPE_DEFINITION_REPRESENTATION ( #1492, #8847 ) ;
#7828 = DIRECTION ( 'NONE',  ( -1.000000000000000000, -2.775557561562891351E-17, 0.000000000000000000 ) ) ;
#7829 = DIRECTION ( 'NONE',  ( 4.625929269271486900E-16, 3.469446951953614978E-15, 1.000000000000000000 ) ) ;
#7830 = CYLINDRICAL_SURFACE ( 'NONE', #15556, 2.649999999999971934 ) ;
#7831 = EDGE_CURVE ( 'NONE', #19104, #21466, #13395, .T. ) ;
#7832 = ORIENTED_EDGE ( 'NONE', *, *, #18645, .T. ) ;
#7833 = ORIENTED_EDGE ( 'NONE', *, *, #1074, .T. ) ;
#7834 = FACE_BOUND ( 'NONE', #3099, .T. ) ;
#7835 = CARTESIAN_POINT ( 'NONE',  ( 72.64999999999999147, -112.6666666666666714, 0.000000000000000000 ) ) ;
#7836 = ADVANCED_FACE ( 'NONE', ( #2362 ), #9627, .F. ) ;
#7837 = EDGE_CURVE ( 'NONE', #14717, #10912, #10165, .T. ) ;
#7838 = AXIS2_PLACEMENT_3D ( 'NONE', #18559, #5649, #12942 ) ;
#7839 = AXIS2_PLACEMENT_3D ( 'NONE', #17961, #23737, #19881 ) ;
#7840 = CARTESIAN_POINT ( 'NONE',  ( 5.000000000000000000, 0.000000000000000000, 0.000000000000000000 ) ) ;
#7841 = EDGE_CURVE ( 'NONE', #8826, #15719, #449, .T. ) ;
#7842 = CARTESIAN_POINT ( 'NONE',  ( -127.8082730365395179, 87.69306101368195527, 27.50000000000646949 ) ) ;
#7843 = PRODUCT_RELATED_PRODUCT_CATEGORY ( 'part', '', ( #10988 ) ) ;
#7844 = ORIENTED_EDGE ( 'NONE', *, *, #2815, .T. ) ;
#7845 = LINE ( 'NONE', #6153, #1746 ) ;
#7846 = ORIENTED_EDGE ( 'NONE', *, *, #11341, .F. ) ;
#7847 = FILL_AREA_STYLE_COLOUR ( '', #13723 ) ;
#7848 = DIRECTION ( 'NONE',  ( 0.000000000000000000, 1.000000000000000000, 0.000000000000000000 ) ) ;
#7849 = VERTEX_POINT ( 'NONE', #18900 ) ;
#7850 = ORIENTED_EDGE ( 'NONE', *, *, #10885, .F. ) ;
#7851 = CARTESIAN_POINT ( 'NONE',  ( 0.6810597143197052450, 4.461075778259290914, -3.598441714920602053 ) ) ;
#7852 = CARTESIAN_POINT ( 'NONE',  ( 0.000000000000000000, 4.685197434473814759, -5.637851296924623057E-15 ) ) ;
#7853=STYLED_ITEM('',(#23934),#12608);
#7854 = DIRECTION ( 'NONE',  ( 0.000000000000000000, -1.000000000000000000, 0.000000000000000000 ) ) ;
#7855 = LINE ( 'NONE', #15238, #18428 ) ;
#7856 = CARTESIAN_POINT ( 'NONE',  ( 0.6511518506208960888, -8.763486134561278007, -7.907570769506051533 ) ) ;
#7857 = CARTESIAN_POINT ( 'NONE',  ( 10.12668159690567649, 0.000000000000000000, -9.999999999999998224 ) ) ;
#7858 = CARTESIAN_POINT ( 'NONE',  ( 2.500000000000000000, 1.178949249685212974, -2.042000000000001148 ) ) ;
#7859 = VERTEX_POINT ( 'NONE', #20583 ) ;
#7860 = DIRECTION ( 'NONE',  ( -1.000000000000000000, 3.495664435217746987E-15, 0.000000000000000000 ) ) ;
#7861 = CARTESIAN_POINT ( 'NONE',  ( -4.203833317240879275, -1.627343821129593859, -3.597273115243890818 ) ) ;
#7862 = FILL_AREA_STYLE ('',( #4235 ) ) ;
#7863 = ORIENTED_EDGE ( 'NONE', *, *, #13767, .F. ) ;
#7864 = DIRECTION ( 'NONE',  ( -0.000000000000000000, 0.000000000000000000, 1.000000000000000000 ) ) ;
#7865 = DIRECTION ( 'NONE',  ( 1.000000000000000000, 0.000000000000000000, 0.000000000000000000 ) ) ;
#7866 = APPLICATION_CONTEXT ( 'automotive_design' ) ;
#7867 = ORIENTED_EDGE ( 'NONE', *, *, #8713, .F. ) ;
#7868 = COLOUR_RGB ( '',1.000000000000000000, 0.9490196078431372140, 0.9098039215686274384 ) ;
#7869 = PLANE ( 'NONE',  #22606 ) ;
#7870 = VECTOR ( 'NONE', #12210, 1000.000000000000000 ) ;
#7871 = EDGE_CURVE ( 'NONE', #6295, #23723, #12897, .T. ) ;
#7872 = EDGE_CURVE ( 'NONE', #18148, #17543, #5525, .T. ) ;
#7873 = ORIENTED_EDGE ( 'NONE', *, *, #623, .T. ) ;
#7874 = ADVANCED_FACE ( 'NONE', ( #2231 ), #7274, .F. ) ;
#7875 = CARTESIAN_POINT ( 'NONE',  ( -146.0000000000004832, -784.4690652294799520, -27.94499999999356632 ) ) ;
#7876 = VERTEX_POINT ( 'NONE', #7555 ) ;
#7877 = DIRECTION ( 'NONE',  ( -1.000000000000000000, -0.000000000000000000, -0.000000000000000000 ) ) ;
#7878 = DIRECTION ( 'NONE',  ( 0.000000000000000000, 0.000000000000000000, 1.000000000000000000 ) ) ;
#7879 = CONTEXT_DEPENDENT_SHAPE_REPRESENTATION ( #8648, #12838 ) ;
#7880 = VERTEX_POINT ( 'NONE', #13169 ) ;
#7881 = CYLINDRICAL_SURFACE ( 'NONE', #4479, 2.649999999999985700 ) ;
#7882 = ORIENTED_EDGE ( 'NONE', *, *, #12035, .F. ) ;
#7883 = CARTESIAN_POINT ( 'NONE',  ( -145.0000000000000284, -5.062647941322544249E-13, 90.00000000000000000 ) ) ;
#7884 = DIRECTION ( 'NONE',  ( -0.000000000000000000, 0.8660254037844391517, 0.4999999999999991673 ) ) ;
#7885 = DIRECTION ( 'NONE',  ( 0.000000000000000000, -1.000000000000000000, -1.110223024625156540E-16 ) ) ;
#7886 = CIRCLE ( 'NONE', #8669, 24.69999999999999929 ) ;
#7887 = VECTOR ( 'NONE', #21423, 1000.000000000000114 ) ;
#7888 = DIRECTION ( 'NONE',  ( -0.000000000000000000, -0.000000000000000000, 1.000000000000000000 ) ) ;
#7889 = ORIENTED_EDGE ( 'NONE', *, *, #7523, .F. ) ;
#7890 = CARTESIAN_POINT ( 'NONE',  ( -280.2488155364688964, 269.9427398886703031, -145.5758453455903805 ) ) ;
#7891 =( NAMED_UNIT ( * ) SI_UNIT ( $, .STERADIAN. ) SOLID_ANGLE_UNIT ( ) );
#7893 = EDGE_LOOP ( 'NONE', ( #21361, #23648, #20024, #11053 ) ) ;
#7892 = EDGE_LOOP ( 'NONE', ( #18868, #4712, #10129, #1230 ) ) ;
#7894 = AXIS2_PLACEMENT_3D ( 'NONE', #22886, #23244, #6472 ) ;
#7895 = CARTESIAN_POINT ( 'NONE',  ( 163.0000000000002558, -801.0618695410406644, -29.99999999999344880 ) ) ;
#7896 = LINE ( 'NONE', #7525, #20741 ) ;
#7897 = CARTESIAN_POINT ( 'NONE',  ( 57.99999999999999289, -56.79999999999999005, 5.199999999999971756 ) ) ;
#7898 = PLANE ( 'NONE',  #1140 ) ;
#7899 = DIRECTION ( 'NONE',  ( -0.000000000000000000, -0.000000000000000000, 1.000000000000000000 ) ) ;
#7900 = ORIENTED_EDGE ( 'NONE', *, *, #12562, .T. ) ;
#7901 = DIRECTION ( 'NONE',  ( -0.000000000000000000, -0.000000000000000000, -1.000000000000000000 ) ) ;
#7902 = FACE_OUTER_BOUND ( 'NONE', #15321, .T. ) ;
#7903 = CARTESIAN_POINT ( 'NONE',  ( 123.1027542345835002, -1094.184478438182623, 31.11216498479339521 ) ) ;
#7904 = ITEM_DEFINED_TRANSFORMATION ( 'NONE', 'NONE', #12777,  #11210 ) ;
#7905 = EDGE_LOOP ( 'NONE', ( #10697, #6070, #4877, #4690 ) ) ;
#7906 = AXIS2_PLACEMENT_3D ( 'NONE', #14632, #9318, #5445 ) ;
#7907 = CARTESIAN_POINT ( 'NONE',  ( 0.000000000000000000, -1000.000000000000000, -150.0000000000000000 ) ) ;
#7908 = ORIENTED_EDGE ( 'NONE', *, *, #21588, .F. ) ;
#7909 = PLANE ( 'NONE',  #7147 ) ;
#7910 = FACE_OUTER_BOUND ( 'NONE', #12309, .T. ) ;
#7911 = EDGE_LOOP ( 'NONE', ( #11886, #14459 ) ) ;
#7912 = CARTESIAN_POINT ( 'NONE',  ( -11.08409875828679247, 22.46856765550231216, -145.0000000000000000 ) ) ;
#7913 = EDGE_LOOP ( 'NONE', ( #1035, #3473, #9732, #23559 ) ) ;
#7914 = CARTESIAN_POINT ( 'NONE',  ( 5.384454397937118664, 0.000000000000000000, -5.000000000000000000 ) ) ;
#7915 = CARTESIAN_POINT ( 'NONE',  ( 2.074729277268262863E-14, -59.80000000000003268, 2.159765843450963423E-13 ) ) ;
#7916 = DIRECTION ( 'NONE',  ( -1.000000000000000000, 0.000000000000000000, 0.000000000000000000 ) ) ;
#7917 = LINE ( 'NONE', #7435, #8635 ) ;
#7918 = CARTESIAN_POINT ( 'NONE',  ( 49.17200000000001836, 0.000000000000000000, 0.000000000000000000 ) ) ;
#7919 = CIRCLE ( 'NONE', #11029, 7.500000000000003553 ) ;
#7920 = DIRECTION ( 'NONE',  ( 1.000000000000000000, 0.000000000000000000, 0.000000000000000000 ) ) ;
#7921 = DIRECTION ( 'NONE',  ( -0.000000000000000000, 1.000000000000000000, 1.224646799147353207E-16 ) ) ;
#7922 = ORIENTED_EDGE ( 'NONE', *, *, #4721, .T. ) ;
#7923 = CARTESIAN_POINT ( 'NONE',  ( -20.00000000000000000, -1000.000000000000000, -150.0000000000000000 ) ) ;
#7924 = LINE ( 'NONE', #9634, #11600 ) ;
#7925 = ORIENTED_EDGE ( 'NONE', *, *, #19898, .F. ) ;
#7926 = ADVANCED_FACE ( 'NONE', ( #20474 ), #12507, .F. ) ;
#7927 = VECTOR ( 'NONE', #13927, 1000.000000000000000 ) ;
#7928 = EDGE_LOOP ( 'NONE', ( #3032, #4402, #9014, #8821 ) ) ;
#7929 = CLOSED_SHELL ( 'NONE', ( #9355, #16700, #15517, #5037, #4391, #14413, #5915, #6938, #17406, #8451, #2225, #20082, #1642, #5958, #2508, #3765, #9150, #19186, #14431, #19939, #5961 ) ) ;
#7930 = CARTESIAN_POINT ( 'NONE',  ( 0.000000000000000000, 0.000000000000000000, 20.00000000000000000 ) ) ;
#7931 = CARTESIAN_POINT ( 'NONE',  ( 0.2500000000000002220, 0.000000000000000000, 2.081668171172168513E-14 ) ) ;
#7933 = CARTESIAN_POINT ( 'NONE',  ( 281.4533442688713194, 269.4578961534455175, -145.6839617489740988 ) ) ;
#7932 = PRODUCT_DEFINITION_SHAPE ( 'NONE', 'NONE',  #23849 ) ;
#7934 = EDGE_CURVE ( 'NONE', #3113, #13794, #23358, .T. ) ;
#7935 = ORIENTED_EDGE ( 'NONE', *, *, #3572, .T. ) ;
#7936 = AXIS2_PLACEMENT_3D ( 'NONE', #6092, #17211, #4288 ) ;
#7937 = FACE_OUTER_BOUND ( 'NONE', #9600, .T. ) ;
#7938 = CARTESIAN_POINT ( 'NONE',  ( 5.000000000000000000, -2.342598717236900718, 4.057500000000001883 ) ) ;
#7939 = ADVANCED_FACE ( 'NONE', ( #23234 ), #10480, .F. ) ;
#7940 = CARTESIAN_POINT ( 'NONE',  ( -121.5574576620399654, 79.04925354955206274, 90.00000000000000000 ) ) ;
#7941 = ORIENTED_EDGE ( 'NONE', *, *, #21647, .T. ) ;
#7942 = CARTESIAN_POINT ( 'NONE',  ( 4.197393957002303999, 7.772902908466098641E-14, -3.503767560748929810 ) ) ;
#7943 = VECTOR ( 'NONE', #12027, 1000.000000000000000 ) ;
#7944 = LINE ( 'NONE', #4436, #11558 ) ;
#7945 = EDGE_CURVE ( 'NONE', #20948, #22842, #7451, .T. ) ;
#7946 =( LENGTH_UNIT ( ) NAMED_UNIT ( * ) SI_UNIT ( .MILLI., .METRE. ) );
#7947 = ORIENTED_EDGE ( 'NONE', *, *, #12443, .T. ) ;
#7948 = LINE ( 'NONE', #10016, #19983 ) ;
#7949 = AXIS2_PLACEMENT_3D ( 'NONE', #23465, #21538, #7046 ) ;
#7950 = CONTEXT_DEPENDENT_SHAPE_REPRESENTATION ( #15433, #12535 ) ;
#7951 = FACE_BOUND ( 'NONE', #19980, .T. ) ;
#7952 = CARTESIAN_POINT ( 'NONE',  ( 99.99999999999987210, -132.2000000000003013, -113.4834095219707848 ) ) ;
#7953 = CARTESIAN_POINT ( 'NONE',  ( 45.00000000000004974, -52.79999999999967031, 50.00000000000018474 ) ) ;
#7954 = VERTEX_POINT ( 'NONE', #13873 ) ;
#7955 = ORIENTED_EDGE ( 'NONE', *, *, #20131, .F. ) ;
#7956 = DIRECTION ( 'NONE',  ( 0.000000000000000000, 1.850371707708594366E-15, 1.000000000000000000 ) ) ;
#7957 = AXIS2_PLACEMENT_3D ( 'NONE', #21872, #9216, #5343 ) ;
#7958 = DIRECTION ( 'NONE',  ( 1.000000000000000000, 0.000000000000000000, 0.000000000000000000 ) ) ;
#7959 = CARTESIAN_POINT ( 'NONE',  ( 2.500000000000000000, 2.357898499370431722, -2.818925648462311528E-15 ) ) ;
#7960 = EDGE_CURVE ( 'NONE', #2349, #603, #5901, .T. ) ;
#7961 = CARTESIAN_POINT ( 'NONE',  ( -127.4426065742858043, 88.22361005463049821, 32.37408494914630097 ) ) ;
#7962 = ORIENTED_EDGE ( 'NONE', *, *, #6269, .T. ) ;
#7963 = DIRECTION ( 'NONE',  ( 1.000000000000000000, 0.000000000000000000, -0.000000000000000000 ) ) ;
#7964 = VERTEX_POINT ( 'NONE', #14100 ) ;
#7965 = B_SPLINE_CURVE_WITH_KNOTS ( 'NONE', 3,
 ( #13142, #425, #2087, #13616, #6208, #2449 ),
 .UNSPECIFIED., .F., .F.,
 ( 4, 2, 4 ),
 ( -5.145455527293010977E-06, 0.0004153350442917342006, 0.0008358155441107593302 ),
 .UNSPECIFIED. ) ;
#7966 = AXIS2_PLACEMENT_3D ( 'NONE', #6922, #14536, #18154 ) ;
#7967 = DIRECTION ( 'NONE',  ( 0.000000000000000000, 0.000000000000000000, 1.000000000000000000 ) ) ;
#7968 = ADVANCED_FACE ( 'NONE', ( #902, #4771 ), #6592, .T. ) ;
#7969 = LINE ( 'NONE', #15120, #9796 ) ;
#7970 = ORIENTED_EDGE ( 'NONE', *, *, #12689, .T. ) ;
#7971 = EDGE_LOOP ( 'NONE', ( #21664, #7315, #19262, #11771 ) ) ;
#7972 = CARTESIAN_POINT ( 'NONE',  ( 20.00000000000000000, 0.000000000000000000, 100.0000000000000000 ) ) ;
#7973 = EDGE_CURVE ( 'NONE', #2180, #2544, #22987, .T. ) ;
#7974 = FACE_OUTER_BOUND ( 'NONE', #6735, .T. ) ;
#7975 = LINE ( 'NONE', #383, #16731 ) ;
#7976 = DIRECTION ( 'NONE',  ( -0.000000000000000000, 1.000000000000000000, -0.000000000000000000 ) ) ;
#7977 = CARTESIAN_POINT ( 'NONE',  ( 16.52066876451827682, -981.1653297051909703, 145.0000119999999981 ) ) ;
#7978 = EDGE_CURVE ( 'NONE', #5513, #8336, #2594, .T. ) ;
#7979 = PRODUCT_DEFINITION ( 'UNKNOWN', '', #10444, #5900 ) ;
#7980 = CARTESIAN_POINT ( 'NONE',  ( -4.000000000000000000, 2.309401076758498483, -5.000000000000000000 ) ) ;
#7981 = ORIENTED_EDGE ( 'NONE', *, *, #12731, .F. ) ;
#7982 = CARTESIAN_POINT ( 'NONE',  ( -6.523606932383669843, -4.893847819345372940, -7.213065638944913260 ) ) ;
#7983 = PRESENTATION_STYLE_ASSIGNMENT (( #7754 ) ) ;
#7984 = EDGE_CURVE ( 'NONE', #14489, #9258, #11824, .T. ) ;
#7985 = AXIS2_PLACEMENT_3D ( 'NONE', #728, #16198, #15848 ) ;
#7986 = ORIENTED_EDGE ( 'NONE', *, *, #898, .F. ) ;
#7987 = DIRECTION ( 'NONE',  ( 1.000000000000000000, 0.000000000000000000, 0.000000000000000000 ) ) ;
#7988 = CIRCLE ( 'NONE', #1794, 7.500000000000005329 ) ;
#7989 = PLANE ( 'NONE',  #11135 ) ;
#7990 = ORIENTED_EDGE ( 'NONE', *, *, #2806, .T. ) ;
#7991 = DIRECTION ( 'NONE',  ( 0.000000000000000000, 0.000000000000000000, -1.000000000000000000 ) ) ;
#7992 = ORIENTED_EDGE ( 'NONE', *, *, #13629, .F. ) ;
#7993 = CARTESIAN_POINT ( 'NONE',  ( 7.500000000000000000, 4.330127018922199866, -1.000000000000000888 ) ) ;
#7994 = DIRECTION ( 'NONE',  ( -1.000000000000000000, 0.000000000000000000, 0.000000000000000000 ) ) ;
#7995 = ORIENTED_EDGE ( 'NONE', *, *, #20321, .F. ) ;
#7996 = EDGE_CURVE ( 'NONE', #4317, #8057, #16327, .T. ) ;
#7997 = CARTESIAN_POINT ( 'NONE',  ( -7.499999999999999112, 34.18698582794336716, -100.0000000000000000 ) ) ;
#7998 = CARTESIAN_POINT ( 'NONE',  ( -194.7500000000000284, -494.4690652294800657, 30.00000000000675726 ) ) ;
#7999 = CIRCLE ( 'NONE', #4118, 5.400000000000002132 ) ;
#8000 = ITEM_DEFINED_TRANSFORMATION ( 'NONE', 'NONE', #11230,  #11210 ) ;
#8001 = ORIENTED_EDGE ( 'NONE', *, *, #16781, .F. ) ;
#8002 =( REPRESENTATION_RELATIONSHIP ('NONE','NONE', #10127, #18083 ) REPRESENTATION_RELATIONSHIP_WITH_TRANSFORMATION ( #4021 )SHAPE_REPRESENTATION_RELATIONSHIP( ) );
#8003 = DIRECTION ( 'NONE',  ( -1.000000000000000000, -0.000000000000000000, -0.000000000000000000 ) ) ;
#8004 = EDGE_CURVE ( 'NONE', #6451, #12251, #10571, .T. ) ;
#8005 = CIRCLE ( 'NONE', #21492, 5.249999999999973355 ) ;
#8006 = CARTESIAN_POINT ( 'NONE',  ( -18.83872056943800288, -983.4834511752143271, -145.0000000000001421 ) ) ;
#8007 = CIRCLE ( 'NONE', #5688, 20.00000000000000000 ) ;
#8008 = FACE_OUTER_BOUND ( 'NONE', #408, .T. ) ;
#8009 = CARTESIAN_POINT ( 'NONE',  ( -10.39117206796836079, 0.000000000000000000, -8.499999999999998224 ) ) ;
#8010 = EDGE_CURVE ( 'NONE', #9561, #17846, #3186, .T. ) ;
#8011 = ORIENTED_EDGE ( 'NONE', *, *, #20811, .T. ) ;
#8012 = CARTESIAN_POINT ( 'NONE',  ( -280.0000000000000000, 273.0000000000000000, -144.9999999999999716 ) ) ;
#8013 = EDGE_CURVE ( 'NONE', #7786, #23662, #15571, .T. ) ;
#8015 = EDGE_LOOP ( 'NONE', ( #12604, #1912 ) ) ;
#8014 = ORIENTED_EDGE ( 'NONE', *, *, #8236, .T. ) ;
#8016 = DIRECTION ( 'NONE',  ( 6.486615240276975916E-15, 2.585650881802458380E-15, -1.000000000000000000 ) ) ;
#8017 = FACE_BOUND ( 'NONE', #3411, .T. ) ;
#8018 = CARTESIAN_POINT ( 'NONE',  ( 131.9719027401102380, 81.29225469460293141, -31.88744336596581519 ) ) ;
#8019 = AXIS2_PLACEMENT_3D ( 'NONE', #8897, #18004, #3430 ) ;
#8020 = FACE_OUTER_BOUND ( 'NONE', #4982, .T. ) ;
#8021 = FACE_OUTER_BOUND ( 'NONE', #6186, .T. ) ;
#8022 = CIRCLE ( 'NONE', #19562, 4.250000000000000000 ) ;
#8023 = VERTEX_POINT ( 'NONE', #12078 ) ;
#8024 = CIRCLE ( 'NONE', #2617, 4.000000000000000000 ) ;
#8025 = CARTESIAN_POINT ( 'NONE',  ( 0.000000000000000000, 0.000000000000000000, -5.000000000000000888 ) ) ;
#8026 = CONICAL_SURFACE ( 'NONE', #19565, 2.059999999999998721, 0.9599310885968738161 ) ;
#8027 = CARTESIAN_POINT ( 'NONE',  ( 45.00000000000000000, 269.9999999999999432, 5.249999999999973355 ) ) ;
#8028 = DIRECTION ( 'NONE',  ( -1.000000000000000000, -0.000000000000000000, -0.000000000000000000 ) ) ;
#8029 = CONTEXT_DEPENDENT_SHAPE_REPRESENTATION ( #8002, #3134 ) ;
#8030 = ORIENTED_EDGE ( 'NONE', *, *, #22440, .T. ) ;
#8031 = DIRECTION ( 'NONE',  ( 0.000000000000000000, -3.495664435217746987E-15, 1.000000000000000000 ) ) ;
#8032 = ORIENTED_EDGE ( 'NONE', *, *, #5584, .F. ) ;
#8034 = EDGE_CURVE ( 'NONE', #11303, #2320, #19390, .T. ) ;
#8033 = CARTESIAN_POINT ( 'NONE',  ( -5.273354073351953256E-15, -59.79999999999976978, 74.99940828143397198 ) ) ;
#8035 = CARTESIAN_POINT ( 'NONE',  ( 137.9031948627977044, -44.80746418436605438, -90.00000000000000000 ) ) ;
#8036 = ORIENTED_EDGE ( 'NONE', *, *, #3305, .F. ) ;
#8037 = CARTESIAN_POINT ( 'NONE',  ( 24.19924082433664125, 6.487720809269068134, -144.9999999999999716 ) ) ;
#8038 = ORIENTED_EDGE ( 'NONE', *, *, #17016, .T. ) ;
#8039 = CARTESIAN_POINT ( 'NONE',  ( 10.00000000000000000, 0.000000000000000000, 0.000000000000000000 ) ) ;
#8040 = DIRECTION ( 'NONE',  ( 0.000000000000000000, -1.000000000000000000, -4.694093751100962712E-16 ) ) ;
#8041 = CARTESIAN_POINT ( 'NONE',  ( 2.500000000000000000, 2.357898499370433054, -1.951563910473907981E-15 ) ) ;
#8042 = CARTESIAN_POINT ( 'NONE',  ( 135.4018704341561374, -51.87806360044677234, 90.00000000000000000 ) ) ;
#8043 = ADVANCED_FACE ( 'NONE', ( #17683 ), #4748, .F. ) ;
#8044 = CIRCLE ( 'NONE', #9198, 145.0000000000000284 ) ;
#8045 = DIRECTION ( 'NONE',  ( 1.000000000000000000, 3.469446951953612710E-16, -5.618537574014070918E-17 ) ) ;
#8046 = AXIS2_PLACEMENT_3D ( 'NONE', #685, #4183, #19026 ) ;
#8047 = EDGE_CURVE ( 'NONE', #2929, #22100, #15549, .T. ) ;
#8048 = CARTESIAN_POINT ( 'NONE',  ( -281.4928932188134354, -127.0000000000000568, -152.4000000000012847 ) ) ;
#8049 = AXIS2_PLACEMENT_3D ( 'NONE', #5893, #112, #16766 ) ;
#8050 = CARTESIAN_POINT ( 'NONE',  ( -7.500000000000000000, -3.160302461882432024, -7.231849989190475725 ) ) ;
#8051 = AXIS2_PLACEMENT_3D ( 'NONE', #9998, #807, #18913 ) ;
#8052 = ADVANCED_FACE ( 'NONE', ( #21316 ), #12182, .T. ) ;
#8053 = ORIENTED_EDGE ( 'NONE', *, *, #23033, .F. ) ;
#8054 = DIRECTION ( 'NONE',  ( 0.000000000000000000, 1.177509268541832635E-16, -1.000000000000000000 ) ) ;
#8055 = CARTESIAN_POINT ( 'NONE',  ( -49.99999999999997158, -62.00000000000001421, 5.199999999999997513 ) ) ;
#8056 = EDGE_LOOP ( 'NONE', ( #3333, #20649, #9145, #22896 ) ) ;
#8057 = VERTEX_POINT ( 'NONE', #1264 ) ;
#8058 = DIRECTION ( 'NONE',  ( -0.000000000000000000, 0.000000000000000000, 1.000000000000000000 ) ) ;
#8059 = DIRECTION ( 'NONE',  ( -1.000000000000000000, -0.000000000000000000, -0.000000000000000000 ) ) ;
#8060 = DIRECTION ( 'NONE',  ( 1.000000000000000000, -0.000000000000000000, 6.982962677686266711E-15 ) ) ;
#8061 = AXIS2_PLACEMENT_3D ( 'NONE', #2386, #20605, #8076 ) ;
#8062 = ORIENTED_EDGE ( 'NONE', *, *, #18614, .F. ) ;
#8064 = AXIS2_PLACEMENT_3D ( 'NONE', #7918, #16852, #315 ) ;
#8063 =( GEOMETRIC_REPRESENTATION_CONTEXT ( 3 ) GLOBAL_UNCERTAINTY_ASSIGNED_CONTEXT ( ( #8856 ) ) GLOBAL_UNIT_ASSIGNED_CONTEXT ( ( #11883, #4355, #10060 ) ) REPRESENTATION_CONTEXT ( 'NONE', 'WORKASPACE' ) );
#8065 = DIRECTION ( 'NONE',  ( -1.000000000000000000, -0.000000000000000000, -0.000000000000000000 ) ) ;
#8066 = CIRCLE ( 'NONE', #3792, 2.055000000000001492 ) ;
#8067 = DIRECTION ( 'NONE',  ( 0.000000000000000000, 0.000000000000000000, -1.000000000000000000 ) ) ;
#8068 = AXIS2_PLACEMENT_3D ( 'NONE', #7191, #1750, #2110 ) ;
#8069 = AXIS2_PLACEMENT_3D ( 'NONE', #17188, #21285, #4734 ) ;
#8070 = FACE_OUTER_BOUND ( 'NONE', #6791, .T. ) ;
#8071 = ORIENTED_EDGE ( 'NONE', *, *, #9329, .F. ) ;
#8072 = CARTESIAN_POINT ( 'NONE',  ( 0.000000000000000000, 0.000000000000000000, -100.0000000000000000 ) ) ;
#8073 = LINE ( 'NONE', #7822, #13503 ) ;
#8074 = CARTESIAN_POINT ( 'NONE',  ( 100.0000000000000000, -1400.000000000000000, -125.0000000000001705 ) ) ;
#8075 = ORIENTED_EDGE ( 'NONE', *, *, #14777, .F. ) ;
#8076 = DIRECTION ( 'NONE',  ( -1.000000000000000000, 0.000000000000000000, 0.000000000000000000 ) ) ;
#8077 = ITEM_DEFINED_TRANSFORMATION ( 'NONE', 'NONE', #12001,  #11210 ) ;
#8078 = LINE ( 'NONE', #4326, #20066 ) ;
#8079 = DIRECTION ( 'NONE',  ( -1.000000000000000000, 1.408839003528726857E-14, 6.982962677686266711E-15 ) ) ;
#8080 = DIRECTION ( 'NONE',  ( -0.000000000000000000, -0.000000000000000000, 1.000000000000000000 ) ) ;
#8081 = ADVANCED_FACE ( 'NONE', ( #6344, #16796, #140, #11036, #12432, #14214, #3742, #14342, #7493 ), #7384, .F. ) ;
#8082 = UNCERTAINTY_MEASURE_WITH_UNIT (LENGTH_MEASURE( 1.000000000000000082E-05 ), #15917, 'distance_accuracy_value', 'NONE');
#8083 = ORIENTED_EDGE ( 'NONE', *, *, #9177, .F. ) ;
#8084 = CIRCLE ( 'NONE', #7662, 2.649999999999971934 ) ;
#8085 = ORIENTED_EDGE ( 'NONE', *, *, #21208, .F. ) ;
#8086 = AXIS2_PLACEMENT_3D ( 'NONE', #1377, #19368, #2827 ) ;
#8087 = FACE_OUTER_BOUND ( 'NONE', #10874, .T. ) ;
#8088 = AXIS2_PLACEMENT_3D ( 'NONE', #16090, #10676, #8726 ) ;
#8089 = DIRECTION ( 'NONE',  ( 0.6964005597823107463, -0.7176533009294141507, 6.982962677686266711E-15 ) ) ;
#8090 = AXIS2_PLACEMENT_3D ( 'NONE', #12181, #2938, #17681 ) ;
#8091 = CIRCLE ( 'NONE', #22333, 5.199999999999982414 ) ;
#8092 =( GEOMETRIC_REPRESENTATION_CONTEXT ( 3 ) GLOBAL_UNCERTAINTY_ASSIGNED_CONTEXT ( ( #19164 ) ) GLOBAL_UNIT_ASSIGNED_CONTEXT ( ( #12282, #17548, #12771 ) ) REPRESENTATION_CONTEXT ( 'NONE', 'WORKASPACE' ) );
#8093 = VECTOR ( 'NONE', #18319, 1000.000000000000000 ) ;
#8094 = B_SPLINE_CURVE_WITH_KNOTS ( 'NONE', 3,
 ( #13447, #13219, #7487, #7606, #20764, #131, #14877, #5562, #5680, #17157, #9800, #4228, #13326, #18949, #12971, #13095, #2412, #614, #20278, #20405 ),
 .UNSPECIFIED., .F., .F.,
 ( 4, 2, 2, 2, 2, 2, 2, 2, 2, 4 ),
 ( 0.000000000000000000, 0.001035985217005892974, 0.002071970434011785947, 0.003107955651017679354, 0.003625948259520565126, 0.004143940868023451331, 0.005179926085029106647, 0.006215911302034762831, 0.007251896519040418147, 0.008287881736046073464 ),
 .UNSPECIFIED. ) ;
#8095 = ORIENTED_EDGE ( 'NONE', *, *, #1831, .F. ) ;
#8096 = CARTESIAN_POINT ( 'NONE',  ( 5.000000000000000000, 0.000000000000000000, 0.000000000000000000 ) ) ;
#8097 = DIRECTION ( 'NONE',  ( 0.000000000000000000, 0.000000000000000000, -1.000000000000000000 ) ) ;
#8098 = ORIENTED_EDGE ( 'NONE', *, *, #5766, .F. ) ;
#8099 = DIRECTION ( 'NONE',  ( 3.736327486719275871E-16, -1.000000000000000000, 3.469446951953614189E-15 ) ) ;
#8100 = ORIENTED_EDGE ( 'NONE', *, *, #16929, .F. ) ;
#8102 = VECTOR ( 'NONE', #7481, 1000.000000000000000 ) ;
#8101 = AXIS2_PLACEMENT_3D ( 'NONE', #6314, #20677, #6207 ) ;
#8103 = CARTESIAN_POINT ( 'NONE',  ( 45.00000000000004974, -52.79999999999967031, 50.00000000000018474 ) ) ;
#8104 = COLOUR_RGB ( '',0.8941176470588234615, 0.8941176470588234615, 0.8941176470588234615 ) ;
#8106 = CONICAL_SURFACE ( 'NONE', #10049, 2.055000000000001492, 0.7853981633974633780 ) ;
#8105 = PLANE ( 'NONE',  #6698 ) ;
#8107 = ORIENTED_EDGE ( 'NONE', *, *, #6466, .T. ) ;
#8108 = ORIENTED_EDGE ( 'NONE', *, *, #16485, .F. ) ;
#8109 = FACE_OUTER_BOUND ( 'NONE', #17856, .T. ) ;
#8110 = VECTOR ( 'NONE', #8963, 1000.000000000000000 ) ;
#8111 = CIRCLE ( 'NONE', #14299, 2.649999999999999467 ) ;
#8112 = LINE ( 'NONE', #7852, #16209 ) ;
#8113 = DIRECTION ( 'NONE',  ( 0.000000000000000000, 0.000000000000000000, 1.000000000000000000 ) ) ;
#8114 = EDGE_CURVE ( 'NONE', #6861, #14389, #16720, .T. ) ;
#8115 = DIRECTION ( 'NONE',  ( -0.000000000000000000, -0.000000000000000000, 1.000000000000000000 ) ) ;
#8116 = EDGE_LOOP ( 'NONE', ( #13521, #17499, #3892, #5904 ) ) ;
#8117 = CARTESIAN_POINT ( 'NONE',  ( 171.6502151485116769, 95.33502053007514121, -32.49999999999322853 ) ) ;
#8118 = ADVANCED_FACE ( 'NONE', ( #5567 ), #19799, .F. ) ;
#8119 = ORIENTED_EDGE ( 'NONE', *, *, #15952, .T. ) ;
#8120 = CIRCLE ( 'NONE', #15012, 7.500000000000004441 ) ;
#8121 = CARTESIAN_POINT ( 'NONE',  ( 287.4000000000013415, -132.2000000000000455, 146.4928932188134638 ) ) ;
#8122 = EDGE_CURVE ( 'NONE', #2147, #21880, #22215, .T. ) ;
#8123 = EDGE_CURVE ( 'NONE', #18606, #21871, #22096, .T. ) ;
#8124 = AXIS2_PLACEMENT_3D ( 'NONE', #3471, #5515, #16394 ) ;
#8125 = AXIS2_PLACEMENT_3D ( 'NONE', #6011, #7828, #15101 ) ;
#8126 = VERTEX_POINT ( 'NONE', #3182 ) ;
#8127 = CARTESIAN_POINT ( 'NONE',  ( 2.500000000000000000, 1.178949249685212974, -2.042000000000001148 ) ) ;
#8128 = ORIENTED_EDGE ( 'NONE', *, *, #15980, .F. ) ;
#8129 = DIRECTION ( 'NONE',  ( -1.000000000000000000, -3.469446951953627008E-16, -3.469446951953616161E-16 ) ) ;
#8130 = CARTESIAN_POINT ( 'NONE',  ( -117.3074641843669781, -85.22886158240918064, -90.00000000000000000 ) ) ;
#8131 = ORIENTED_EDGE ( 'NONE', *, *, #1775, .T. ) ;
#8132 = EDGE_CURVE ( 'NONE', #14202, #404, #18624, .T. ) ;
#8133 = CARTESIAN_POINT ( 'NONE',  ( -280.2488155364689533, 272.8646579186752774, 146.3610889986682935 ) ) ;
#8134 = FACE_OUTER_BOUND ( 'NONE', #3958, .T. ) ;
#8135 = VERTEX_POINT ( 'NONE', #18593 ) ;
#8136 = B_SPLINE_CURVE_WITH_KNOTS ( 'NONE', 3,
 ( #11874, #18073, #8919, #14820, #1529, #3558 ),
 .UNSPECIFIED., .F., .F.,
 ( 4, 2, 4 ),
 ( 2.475503369207376426E-07, 0.002222330217055627170, 0.004444412883774334112 ),
 .UNSPECIFIED. ) ;
#8137 = LINE ( 'NONE', #409, #21054 ) ;
#8138 = ORIENTED_EDGE ( 'NONE', *, *, #15235, .F. ) ;
#8139 = LINE ( 'NONE', #17065, #19402 ) ;
#8140 = FACE_OUTER_BOUND ( 'NONE', #5575, .T. ) ;
#8141 = CARTESIAN_POINT ( 'NONE',  ( 0.000000000000000000, 0.000000000000000000, 0.000000000000000000 ) ) ;
#8142 = ORIENTED_EDGE ( 'NONE', *, *, #3515, .F. ) ;
#8143 = CARTESIAN_POINT ( 'NONE',  ( -280.8708543776411943, 269.1333820183295416, -146.7350371479512887 ) ) ;
#8144 = PRODUCT_DEFINITION_SHAPE ( 'NONE', 'NONE',  #23871 ) ;
#8146 = EDGE_LOOP ( 'NONE', ( #7685, #979 ) ) ;
#8145 = ORIENTED_EDGE ( 'NONE', *, *, #5155, .F. ) ;
#8147 = DIRECTION ( 'NONE',  ( -1.000000000000000000, 0.000000000000000000, -6.982962677686266711E-15 ) ) ;
#8148 = CARTESIAN_POINT ( 'NONE',  ( 7.915340744421234476, 3.857466640755322640, -7.913699667209310284 ) ) ;
#8149 = CARTESIAN_POINT ( 'NONE',  ( 2.500000000000015987, 1.768423874527823347, -1.021000000000001018 ) ) ;
#8150 = EDGE_CURVE ( 'NONE', #3718, #22067, #21844, .T. ) ;
#8151 = EDGE_CURVE ( 'NONE', #8135, #23656, #3979, .T. ) ;
#8152 = CARTESIAN_POINT ( 'NONE',  ( 281.7592670532758916, 269.1520027839447948, 145.8708543776412228 ) ) ;
#8153 = FACE_OUTER_BOUND ( 'NONE', #21023, .T. ) ;
#8154 = EDGE_CURVE ( 'NONE', #9872, #11044, #7192, .T. ) ;
#8155 = VERTEX_POINT ( 'NONE', #11393 ) ;
#8156 = FACE_OUTER_BOUND ( 'NONE', #8430, .T. ) ;
#8157 = EDGE_CURVE ( 'NONE', #17523, #20328, #37, .T. ) ;
#8158 = ADVANCED_FACE ( 'NONE', ( #20284 ), #17931, .F. ) ;
#8159 = CARTESIAN_POINT ( 'NONE',  ( -285.2000000000006708, 90.00000000000102318, -35.00000000000001421 ) ) ;
#8160 = EDGE_CURVE ( 'NONE', #12572, #4754, #16457, .T. ) ;
#8161 = CYLINDRICAL_SURFACE ( 'NONE', #13917, 2.199999999999979750 ) ;
#8162 = CONTEXT_DEPENDENT_SHAPE_REPRESENTATION ( #3049, #22782 ) ;
#8163 = ORIENTED_EDGE ( 'NONE', *, *, #16430, .T. ) ;
#8164 = DIRECTION ( 'NONE',  ( -0.000000000000000000, 0.000000000000000000, -1.000000000000000000 ) ) ;
#8165 = ORIENTED_EDGE ( 'NONE', *, *, #14060, .F. ) ;
#8166 = FACE_OUTER_BOUND ( 'NONE', #17965, .T. ) ;
#8167 = CARTESIAN_POINT ( 'NONE',  ( 5.200000000000002842, 0.000000000000000000, 0.000000000000000000 ) ) ;
#8168 = ORIENTED_EDGE ( 'NONE', *, *, #7300, .T. ) ;
#8169 = CARTESIAN_POINT ( 'NONE',  ( -24.83992656990903569, 3.266860234290754672, -145.0000000000000000 ) ) ;
#8170 = ORIENTED_EDGE ( 'NONE', *, *, #4635, .T. ) ;
#8171 = FILL_AREA_STYLE ('',( #793 ) ) ;
#8172 = CARTESIAN_POINT ( 'NONE',  ( 2.100000000000000089, 0.000000000000000000, -5.000000000000000000 ) ) ;
#8173 = DIRECTION ( 'NONE',  ( 1.000000000000000000, 0.000000000000000000, 0.000000000000000000 ) ) ;
#8174 = DIRECTION ( 'NONE',  ( 0.000000000000000000, -0.5000000000000009992, -0.8660254037844380415 ) ) ;
#8175 = DIRECTION ( 'NONE',  ( 1.000000000000000000, -3.051161311199799893E-31, -8.144298233840332611E-17 ) ) ;
#8176 = DIRECTION ( 'NONE',  ( -1.000000000000000000, -0.000000000000000000, -0.000000000000000000 ) ) ;
#8177 = CARTESIAN_POINT ( 'NONE',  ( -2.700000000000001066, 0.000000000000000000, 0.000000000000000000 ) ) ;
#8178 = EDGE_LOOP ( 'NONE', ( #15258, #23028, #17791, #15730 ) ) ;
#8179 =( NAMED_UNIT ( * ) SI_UNIT ( $, .STERADIAN. ) SOLID_ANGLE_UNIT ( ) );
#8180 = DIRECTION ( 'NONE',  ( 1.000000000000000000, 0.000000000000000000, 0.000000000000000000 ) ) ;
#8181 = CARTESIAN_POINT ( 'NONE',  ( 2.500000000000000000, -1.178949249685213863, 2.042000000000002924 ) ) ;
#8182 = ORIENTED_EDGE ( 'NONE', *, *, #2311, .T. ) ;
#8183 = EDGE_LOOP ( 'NONE', ( #18066, #7254, #20038, #4485, #16729, #23563, #10348, #1275, #22349, #7539, #19190, #14849 ) ) ;
#8184 = FACE_OUTER_BOUND ( 'NONE', #2760, .T. ) ;
#8185 = DIRECTION ( 'NONE',  ( 1.000000000000000000, 0.000000000000000000, 0.000000000000000000 ) ) ;
#8186 = ADVANCED_BREP_SHAPE_REPRESENTATION ( '', ( #11885, #11210 ), #22754 ) ;
#8187 = CARTESIAN_POINT ( 'NONE',  ( 194.7499999999997726, -209.9999999999996874, 27.50000000000675371 ) ) ;
#8188 = EDGE_CURVE ( 'NONE', #3982, #21618, #15325, .T. ) ;
#8189 = EDGE_CURVE ( 'NONE', #15959, #7096, #1943, .T. ) ;
#8190 = PLANE ( 'NONE',  #4956 ) ;
#8191 = ADVANCED_FACE ( 'NONE', ( #20410 ), #16568, .F. ) ;
#8192 = DIRECTION ( 'NONE',  ( 0.000000000000000000, 0.000000000000000000, 1.000000000000000000 ) ) ;
#8193 = LINE ( 'NONE', #10128, #12742 ) ;
#8194 = ORIENTED_EDGE ( 'NONE', *, *, #18134, .F. ) ;
#8195 = CYLINDRICAL_SURFACE ( 'NONE', #970, 2.500000000000002220 ) ;
#8196 = DIRECTION ( 'NONE',  ( 0.000000000000000000, 0.000000000000000000, 1.000000000000000000 ) ) ;
#8197 = CARTESIAN_POINT ( 'NONE',  ( 158.0000000000000284, -500.0000000000000000, -29.99999999999997158 ) ) ;
#8198 = ORIENTED_EDGE ( 'NONE', *, *, #11315, .T. ) ;
#8199 = DIRECTION ( 'NONE',  ( -5.478074134663601247E-16, 1.000000000000000000, 0.000000000000000000 ) ) ;
#8200 = DIRECTION ( 'NONE',  ( 1.000000000000000000, 0.000000000000000000, 0.000000000000000000 ) ) ;
#8201 = LINE ( 'NONE', #10139, #359 ) ;
#8202 = DIRECTION ( 'NONE',  ( 1.000000000000000000, 0.000000000000000000, 0.000000000000000000 ) ) ;
#8203 = AXIS2_PLACEMENT_3D ( 'NONE', #5645, #18659, #14598 ) ;
#8204 = ORIENTED_EDGE ( 'NONE', *, *, #18577, .T. ) ;
#8205 = ORIENTED_EDGE ( 'NONE', *, *, #13014, .T. ) ;
#8206 = DIRECTION ( 'NONE',  ( 0.000000000000000000, 0.000000000000000000, -1.000000000000000000 ) ) ;
#8207 = CARTESIAN_POINT ( 'NONE',  ( -25.00000000000000000, 1.865214261513747767E-15, 138.9999999999999716 ) ) ;
#8208 = ORIENTED_EDGE ( 'NONE', *, *, #20877, .F. ) ;
#8209 = ORIENTED_EDGE ( 'NONE', *, *, #22002, .T. ) ;
#8210 = CARTESIAN_POINT ( 'NONE',  ( -102.3500000000000085, -29.99999999999998579, 3.000000000000001332 ) ) ;
#8211 = LINE ( 'NONE', #19301, #11887 ) ;
#8212 = ORIENTED_EDGE ( 'NONE', *, *, #6949, .F. ) ;
#8213 = CARTESIAN_POINT ( 'NONE',  ( 24.99999999999999645, 2.463415629691065208E-15, 145.0000059999999849 ) ) ;
#8214 = VECTOR ( 'NONE', #12716, 999.9999999999998863 ) ;
#8215 = ORIENTED_EDGE ( 'NONE', *, *, #279, .T. ) ;
#8216 = CARTESIAN_POINT ( 'NONE',  ( -5.883060564508084174E-15, -56.79999999999977689, 73.75676759431468099 ) ) ;
#8217 = FACE_OUTER_BOUND ( 'NONE', #21040, .T. ) ;
#8218 = ORIENTED_EDGE ( 'NONE', *, *, #9100, .T. ) ;
#8219 = ORIENTED_EDGE ( 'NONE', *, *, #1512, .F. ) ;
#8220 = DIRECTION ( 'NONE',  ( 0.000000000000000000, 0.000000000000000000, 1.000000000000000000 ) ) ;
#8221 = DIRECTION ( 'NONE',  ( 1.000000000000000000, 0.000000000000000000, 0.000000000000000000 ) ) ;
#8222 = FACE_OUTER_BOUND ( 'NONE', #18774, .T. ) ;
#8223 = CARTESIAN_POINT ( 'NONE',  ( -1.500000000000000000, 11.99999999999999822, 200.2421591959677016 ) ) ;
#8224 = ORIENTED_EDGE ( 'NONE', *, *, #4932, .T. ) ;
#8225 = CARTESIAN_POINT ( 'NONE',  ( 20.00000000000000000, 0.000000000000000000, -150.0000000000000000 ) ) ;
#8226 = FILL_AREA_STYLE ('',( #10417 ) ) ;
#8227 = VECTOR ( 'NONE', #4923, 1000.000000000000000 ) ;
#8228 = EDGE_LOOP ( 'NONE', ( #22078, #21384 ) ) ;
#8229 = EDGE_CURVE ( 'NONE', #20414, #20433, #13812, .T. ) ;
#8230 = EDGE_LOOP ( 'NONE', ( #19614, #3056, #18369 ) ) ;
#8231 = CARTESIAN_POINT ( 'NONE',  ( -281.4928932188134354, -132.2000000000000455, -152.4000000000012562 ) ) ;
#8232 = EDGE_LOOP ( 'NONE', ( #11664, #23713 ) ) ;
#8233 = CARTESIAN_POINT ( 'NONE',  ( 7.500000000000000000, -5.637851296924623057E-15, -6.991905250253753756 ) ) ;
#8234 = FACE_BOUND ( 'NONE', #12232, .T. ) ;
#8235 = ORIENTED_EDGE ( 'NONE', *, *, #8556, .F. ) ;
#8236 = EDGE_CURVE ( 'NONE', #10799, #2037, #22461, .T. ) ;
#8237 = COLOUR_RGB ( '',0.8941176470588234615, 0.8941176470588234615, 0.8941176470588234615 ) ;
#8238 = CARTESIAN_POINT ( 'NONE',  ( -280.1244295015776515, 273.0299999999999159, 145.6847249064869629 ) ) ;
#8239 = LINE ( 'NONE', #17780, #11789 ) ;
#8240 = EDGE_CURVE ( 'NONE', #3749, #10625, #23009, .T. ) ;
#8241 = ORIENTED_EDGE ( 'NONE', *, *, #12011, .F. ) ;
#8242 = AXIS2_PLACEMENT_3D ( 'NONE', #9557, #20528, #23480 ) ;
#8243 = DIRECTION ( 'NONE',  ( -0.000000000000000000, 0.000000000000000000, -1.000000000000000000 ) ) ;
#8244 = CARTESIAN_POINT ( 'NONE',  ( -25.00004926070572964, -998.3579766119668193, -145.0000000000001137 ) ) ;
#8245 = EDGE_CURVE ( 'NONE', #6599, #12056, #4896, .T. ) ;
#8246 = CARTESIAN_POINT ( 'NONE',  ( -7.922281120364393914, 4.573931137438271399, -8.047472243342930653 ) ) ;
#8247 = DIRECTION ( 'NONE',  ( -1.000000000000000000, -0.000000000000000000, -0.000000000000000000 ) ) ;
#8248 = ORIENTED_EDGE ( 'NONE', *, *, #23370, .T. ) ;
#8249 = CARTESIAN_POINT ( 'NONE',  ( 146.4450000000002206, -801.0618695410406644, -27.49999999999356604 ) ) ;
#8250 = ITEM_DEFINED_TRANSFORMATION ( 'NONE', 'NONE', #21957,  #11210 ) ;
#8251 = VECTOR ( 'NONE', #7823, 1000.000000000000000 ) ;
#8253 = ORIENTED_EDGE ( 'NONE', *, *, #10889, .T. ) ;
#8252 = ORIENTED_EDGE ( 'NONE', *, *, #3031, .F. ) ;
#8254 = AXIS2_PLACEMENT_3D ( 'NONE', #11088, #18409, #4034 ) ;
#8255 = DIRECTION ( 'NONE',  ( -6.982962677686266711E-15, 9.837870180509810443E-29, -1.000000000000000000 ) ) ;
#8256 = CARTESIAN_POINT ( 'NONE',  ( 7.500000000000000888, -4.651016565836964212, -7.928861822685564498 ) ) ;
#8257 = DIRECTION ( 'NONE',  ( 0.000000000000000000, 0.000000000000000000, 1.000000000000000000 ) ) ;
#8258 = LINE ( 'NONE', #22849, #10813 ) ;
#8259 = CARTESIAN_POINT ( 'NONE',  ( -282.6188186979287025, 272.3436892194421262, -145.4976310729377929 ) ) ;
#8260 = VERTEX_POINT ( 'NONE', #4234 ) ;
#8261 = CARTESIAN_POINT ( 'NONE',  ( 7.500000000000000888, -3.640541674360523228, -0.7158139487964624292 ) ) ;
#8262 = FACE_BOUND ( 'NONE', #18677, .T. ) ;
#8263 = DIRECTION ( 'NONE',  ( -0.000000000000000000, -1.000000000000000000, -1.110223024625156540E-16 ) ) ;
#8264 = ITEM_DEFINED_TRANSFORMATION ( 'NONE', 'NONE', #11593,  #11210 ) ;
#8265 = ORIENTED_EDGE ( 'NONE', *, *, #12978, .T. ) ;
#8267 = DIRECTION ( 'NONE',  ( 0.000000000000000000, -1.000000000000000000, -5.286776307738891306E-15 ) ) ;
#8266 = AXIS2_PLACEMENT_3D ( 'NONE', #13554, #10133, #15681 ) ;
#8268 = ADVANCED_FACE ( 'NONE', ( #13333 ), #13457, .F. ) ;
#8269 = EDGE_LOOP ( 'NONE', ( #10486, #22728, #10878, #14473 ) ) ;
#8270 = DIRECTION ( 'NONE',  ( 0.000000000000000000, 1.177509268541832635E-16, -1.000000000000000000 ) ) ;
#8271 = VECTOR ( 'NONE', #21547, 1000.000000000000000 ) ;
#8272 = CARTESIAN_POINT ( 'NONE',  ( 10.40000000000000036, 0.000000000000000000, -5.400000000000002132 ) ) ;
#8273 = ORIENTED_EDGE ( 'NONE', *, *, #15346, .T. ) ;
#8274 = CARTESIAN_POINT ( 'NONE',  ( -23.72528575881786850, 8.050112875934637202, -145.0000000000000000 ) ) ;
#8275 = EDGE_CURVE ( 'NONE', #16958, #6562, #18013, .T. ) ;
#8276 = ORIENTED_EDGE ( 'NONE', *, *, #19191, .F. ) ;
#8277 = AXIS2_PLACEMENT_3D ( 'NONE', #20506, #5902, #6150 ) ;
#8278 = SURFACE_STYLE_FILL_AREA ( #8171 ) ;
#8279 = CARTESIAN_POINT ( 'NONE',  ( -44.99999999999997868, -56.79999999999935767, 197.6500000000001478 ) ) ;
#8280 = ADVANCED_FACE ( 'NONE', ( #20771 ), #13589, .T. ) ;
#8281 = FACE_OUTER_BOUND ( 'NONE', #4257, .T. ) ;
#8282 = DIRECTION ( 'NONE',  ( 1.000000000000000000, 0.000000000000000000, 0.000000000000000000 ) ) ;
#8283 = CARTESIAN_POINT ( 'NONE',  ( 80.00000000000000000, -56.80000000000000426, 2.010073102693556962E-13 ) ) ;
#8284 = DIRECTION ( 'NONE',  ( 1.000000000000000000, 0.000000000000000000, 0.000000000000000000 ) ) ;
#8285 = EDGE_CURVE ( 'NONE', #442, #14560, #9928, .T. ) ;
#8286 = ORIENTED_EDGE ( 'NONE', *, *, #9789, .F. ) ;
#8287 = AXIS2_PLACEMENT_3D ( 'NONE', #21056, #17329, #6687 ) ;
#8288 = CARTESIAN_POINT ( 'NONE',  ( 5.000000000000000888, 0.000000000000000000, 0.000000000000000000 ) ) ;
#8289 = LINE ( 'NONE', #17570, #14679 ) ;
#8290 = ORIENTED_EDGE ( 'NONE', *, *, #2513, .T. ) ;
#8291 = ORIENTED_EDGE ( 'NONE', *, *, #21394, .T. ) ;
#8292 = LINE ( 'NONE', #8403, #21936 ) ;
#8294 = AXIS2_PLACEMENT_3D ( 'NONE', #20831, #4518, #8267 ) ;
#8293 = CARTESIAN_POINT ( 'NONE',  ( -79.99999999999995737, -62.00000000000004263, 3.000000000000000000 ) ) ;
#8295 = CARTESIAN_POINT ( 'NONE',  ( 2.500000000000002220, -1.178949249685215417, 2.042000000000002036 ) ) ;
#8296 = AXIS2_PLACEMENT_3D ( 'NONE', #18007, #14407, #1929 ) ;
#8297 = AXIS2_PLACEMENT_3D ( 'NONE', #19271, #2740, #10124 ) ;
#8298 = CARTESIAN_POINT ( 'NONE',  ( 4.101954839143059139, -2.368264730582948285, -3.681130640444269631 ) ) ;
#8299 = DIRECTION ( 'NONE',  ( 0.000000000000000000, 1.000000000000000000, 0.000000000000000000 ) ) ;
#8300 = CARTESIAN_POINT ( 'NONE',  ( -10.39117206796836257, 1.272551561242683764E-15, -8.499999999999998224 ) ) ;
#8301 = ORIENTED_EDGE ( 'NONE', *, *, #21900, .F. ) ;
#8302 = DIRECTION ( 'NONE',  ( 0.000000000000000000, -0.5000000000000011102, -0.8660254037844379305 ) ) ;
#8303 = CARTESIAN_POINT ( 'NONE',  ( 2.500000000000000000, -1.178949249685213863, 2.042000000000001148 ) ) ;
#8304 = DIRECTION ( 'NONE',  ( 1.000000000000000000, 0.000000000000000000, 0.000000000000000000 ) ) ;
#8305 = EDGE_LOOP ( 'NONE', ( #16513, #18232, #18710, #7240 ) ) ;
#8306 = DIRECTION ( 'NONE',  ( 0.000000000000000000, 0.000000000000000000, -1.000000000000000000 ) ) ;
#8307 = CIRCLE ( 'NONE', #5213, 5.249999999999956479 ) ;
#8308 = PLANE ( 'NONE',  #14314 ) ;
#8309 = DIRECTION ( 'NONE',  ( -0.7071067811865320296, 9.875400524328840493E-15, 0.7071067811865631159 ) ) ;
#8310 = CYLINDRICAL_SURFACE ( 'NONE', #7060, 7.500000000000007105 ) ;
#8311 = ORIENTED_EDGE ( 'NONE', *, *, #1825, .F. ) ;
#8313 = VERTEX_POINT ( 'NONE', #8225 ) ;
#8312 = ADVANCED_FACE ( 'NONE', ( #2301 ), #3252, .F. ) ;
#8314 = DIRECTION ( 'NONE',  ( -1.000000000000000000, 3.495664435217746987E-15, 0.000000000000000000 ) ) ;
#8315 = LINE ( 'NONE', #17487, #7313 ) ;
#8316 = EDGE_CURVE ( 'NONE', #11691, #6889, #6174, .T. ) ;
#8317 = ORIENTED_EDGE ( 'NONE', *, *, #13798, .T. ) ;
#8318 = CIRCLE ( 'NONE', #13349, 7.500000000000004441 ) ;
#8319 = ORIENTED_EDGE ( 'NONE', *, *, #16272, .F. ) ;
#8320 = DIRECTION ( 'NONE',  ( 0.000000000000000000, -0.000000000000000000, 1.000000000000000000 ) ) ;
#8321 = CARTESIAN_POINT ( 'NONE',  ( -126.9537165176732287, 88.92563123478208809, 31.88926668738024972 ) ) ;
#8322 = VERTEX_POINT ( 'NONE', #4597 ) ;
#8323 = CARTESIAN_POINT ( 'NONE',  ( -135.0388036711515838, -1076.089031023631605, -31.99040335529160117 ) ) ;
#8324 = VECTOR ( 'NONE', #13383, 1000.000000000000000 ) ;
#8325 = ORIENTED_EDGE ( 'NONE', *, *, #22785, .F. ) ;
#8326 = DIRECTION ( 'NONE',  ( -1.000000000000000000, -2.775557561562891351E-17, 0.000000000000000000 ) ) ;
#8327 = DIRECTION ( 'NONE',  ( -0.000000000000000000, -0.000000000000000000, 1.000000000000000000 ) ) ;
#8328 = VERTEX_POINT ( 'NONE', #2538 ) ;
#8329 = EDGE_LOOP ( 'NONE', ( #5590, #1313, #14140, #11197 ) ) ;
#8330 = DIRECTION ( 'NONE',  ( 1.000000000000000000, 0.000000000000000000, 0.000000000000000000 ) ) ;
#8331 = PRODUCT_DEFINITION_SHAPE ( 'NONE', 'NONE',  #23876 ) ;
#8332 = CARTESIAN_POINT ( 'NONE',  ( 4.236525694536557474, -2.416953475386482530, -3.751298745799839462 ) ) ;
#8333 = CONICAL_SURFACE ( 'NONE', #13768, 2.055000000000001492, 0.7853981633974633780 ) ;
#8334 = DIRECTION ( 'NONE',  ( -0.000000000000000000, -0.000000000000000000, -1.000000000000000000 ) ) ;
#8335 = FACE_OUTER_BOUND ( 'NONE', #18064, .T. ) ;
#8336 = VERTEX_POINT ( 'NONE', #12016 ) ;
#8337 = ADVANCED_FACE ( 'NONE', ( #19317 ), #17285, .F. ) ;
#8338 = PLANE ( 'NONE',  #11091 ) ;
#8339 = SHAPE_REPRESENTATION_RELATIONSHIP ( 'NONE' , 'NONE' ,  #21947, #8186 ) ;
#8340 = ORIENTED_EDGE ( 'NONE', *, *, #14633, .F. ) ;
#8341 = EDGE_CURVE ( 'NONE', #21062, #5386, #17767, .T. ) ;
#8342 = ORIENTED_EDGE ( 'NONE', *, *, #23734, .T. ) ;
#8343 = CARTESIAN_POINT ( 'NONE',  ( 34.75000000000003553, 100.0000000000000000, 150.2000000000009550 ) ) ;
#8344 = ORIENTED_EDGE ( 'NONE', *, *, #16367, .T. ) ;
#8345 = VECTOR ( 'NONE', #1241, 1000.000000000000000 ) ;
#8346 = DIRECTION ( 'NONE',  ( 0.000000000000000000, 0.4999999999999989453, -0.8660254037844393737 ) ) ;
#8347 = CARTESIAN_POINT ( 'NONE',  ( -144.8060344827586619, 7.497491405671214082, -90.00000000000000000 ) ) ;
#8348 = EDGE_LOOP ( 'NONE', ( #20676, #22808 ) ) ;
#8349 = VECTOR ( 'NONE', #10605, 1000.000000000000000 ) ;
#8350 = CARTESIAN_POINT ( 'NONE',  ( -280.6220388411723548, 271.9582675804705332, 148.1956429438695579 ) ) ;
#8351 = CARTESIAN_POINT ( 'NONE',  ( 0.000000000000000000, 0.000000000000000000, 0.000000000000000000 ) ) ;
#8352 = VERTEX_POINT ( 'NONE', #19424 ) ;
#8353 = FACE_OUTER_BOUND ( 'NONE', #19074, .T. ) ;
#8354 = CARTESIAN_POINT ( 'NONE',  ( -24.99999999999998224, -1000.000000000000000, -145.0000060000000417 ) ) ;
#8355 = VECTOR ( 'NONE', #5084, 1000.000000000000000 ) ;
#8356 = DIRECTION ( 'NONE',  ( -0.000000000000000000, -0.000000000000000000, 1.000000000000000000 ) ) ;
#8357 = EDGE_CURVE ( 'NONE', #19560, #21767, #21371, .T. ) ;
#8358 = ADVANCED_FACE ( 'NONE', ( #8823 ), #14399, .F. ) ;
#8359 = LINE ( 'NONE', #11670, #23481 ) ;
#8360 = ORIENTED_EDGE ( 'NONE', *, *, #13203, .F. ) ;
#8361 = CARTESIAN_POINT ( 'NONE',  ( 312.2000000000013529, -132.2000000000000455, 146.4928932188134638 ) ) ;
#8362 = VECTOR ( 'NONE', #18123, 1000.000000000000000 ) ;
#8363 = PRESENTATION_STYLE_ASSIGNMENT (( #981 ) ) ;
#8365 = ORIENTED_EDGE ( 'NONE', *, *, #17356, .F. ) ;
#8364 = VERTEX_POINT ( 'NONE', #23296 ) ;
#8366 = ADVANCED_FACE ( 'NONE', ( #4832 ), #14290, .T. ) ;
#8367 = CARTESIAN_POINT ( 'NONE',  ( 0.000000000000000000, 0.000000000000000000, 142.0000000000000568 ) ) ;
#8368 = CARTESIAN_POINT ( 'NONE',  ( 7.499999999999999112, 3.105728215500122680, -7.659336188854854122 ) ) ;
#8369 = LINE ( 'NONE', #21399, #8516 ) ;
#8370 = PLANE ( 'NONE',  #15022 ) ;
#8371 = CARTESIAN_POINT ( 'NONE',  ( 20.00000000000000000, 0.000000000000000000, -100.0000000000000000 ) ) ;
#8372 = CARTESIAN_POINT ( 'NONE',  ( -280.0000000000000568, 272.9999999999999432, -144.9999999999999716 ) ) ;
#8373 = ORIENTED_EDGE ( 'NONE', *, *, #14175, .T. ) ;
#8374 = EDGE_CURVE ( 'NONE', #15690, #22268, #23185, .T. ) ;
#8375 = CIRCLE ( 'NONE', #19931, 145.0000000000000284 ) ;
#8376 = FACE_OUTER_BOUND ( 'NONE', #15469, .T. ) ;
#8377 = DIRECTION ( 'NONE',  ( -1.000000000000000000, -0.000000000000000000, -0.000000000000000000 ) ) ;
#8378 = LINE ( 'NONE', #10204, #22336 ) ;
#8379 = CONTEXT_DEPENDENT_SHAPE_REPRESENTATION ( #1683, #16263 ) ;
#8380 = VERTEX_POINT ( 'NONE', #12241 ) ;
#8381 = DIRECTION ( 'NONE',  ( 2.238759164535664589E-46, 3.469446951953614189E-15, 1.000000000000000000 ) ) ;
#8382 = ORIENTED_EDGE ( 'NONE', *, *, #10080, .F. ) ;
#8383 = CYLINDRICAL_SURFACE ( 'NONE', #760, 2.500000000000000444 ) ;
#8384 = LINE ( 'NONE', #15761, #21433 ) ;
#8385 = ORIENTED_EDGE ( 'NONE', *, *, #7402, .T. ) ;
#8386 = DIRECTION ( 'NONE',  ( 0.000000000000000000, 0.000000000000000000, 1.000000000000000000 ) ) ;
#8387 = DIRECTION ( 'NONE',  ( -1.000000000000000000, -0.000000000000000000, -0.000000000000000000 ) ) ;
#8388 = LINE ( 'NONE', #21072, #3240 ) ;
#8389 = CARTESIAN_POINT ( 'NONE',  ( 282.1433523009092710, 268.3743436287468853, 146.2447782964894714 ) ) ;
#8390 = DIRECTION ( 'NONE',  ( -1.000000000000000000, -0.000000000000000000, -0.000000000000000000 ) ) ;
#8391 = CIRCLE ( 'NONE', #11486, 5.249999999999991118 ) ;
#8392 = DIRECTION ( 'NONE',  ( -6.753181414994864868E-15, 6.753181414994864868E-15, -1.000000000000000000 ) ) ;
#8393 = VERTEX_POINT ( 'NONE', #23418 ) ;
#8394 = EDGE_CURVE ( 'NONE', #12953, #14948, #19545, .T. ) ;
#8395 = FILL_AREA_STYLE_COLOUR ( '', #10026 ) ;
#8396 = EDGE_CURVE ( 'NONE', #18735, #13410, #10416, .T. ) ;
#8397 = DIRECTION ( 'NONE',  ( -0.000000000000000000, -0.000000000000000000, 1.000000000000000000 ) ) ;
#8398 = DIRECTION ( 'NONE',  ( 1.000000000000000000, 0.000000000000000000, 0.000000000000000000 ) ) ;
#8399 = AXIS2_PLACEMENT_3D ( 'NONE', #10800, #15131, #11392 ) ;
#8400 = ORIENTED_EDGE ( 'NONE', *, *, #21599, .T. ) ;
#8401 = ORIENTED_EDGE ( 'NONE', *, *, #9042, .T. ) ;
#8402 = AXIS2_PLACEMENT_3D ( 'NONE', #23634, #7093, #21819 ) ;
#8403 = CARTESIAN_POINT ( 'NONE',  ( 79.04925354955338435, -121.5574576620390843, -2.775557561562891351E-14 ) ) ;
#8404 = DIRECTION ( 'NONE',  ( 0.000000000000000000, 0.000000000000000000, 1.000000000000000000 ) ) ;
#8405 = EDGE_CURVE ( 'NONE', #7615, #13673, #8375, .T. ) ;
#8406 = DIRECTION ( 'NONE',  ( 0.000000000000000000, 1.000000000000000000, 0.000000000000000000 ) ) ;
#8407 = ADVANCED_FACE ( 'NONE', ( #3140 ), #3363, .F. ) ;
#8408 = LINE ( 'NONE', #10356, #13091 ) ;
#8409 = CARTESIAN_POINT ( 'NONE',  ( 2.999999999999995559, 0.000000000000000000, 0.000000000000000000 ) ) ;
#8410 = AXIS2_PLACEMENT_3D ( 'NONE', #7196, #14585, #5405 ) ;
#8411 = B_SPLINE_CURVE_WITH_KNOTS ( 'NONE', 3,
 ( #22949, #5094, #14173, #17524, #19561, #17889 ),
 .UNSPECIFIED., .F., .F.,
 ( 4, 2, 4 ),
 ( 0.002365888236227977302, 0.003551327329835078910, 0.004736766423442180518 ),
 .UNSPECIFIED. ) ;
#8412 = CARTESIAN_POINT ( 'NONE',  ( 0.2727178028658734932, 0.000000000000000000, 0.000000000000000000 ) ) ;
#8413 = ORIENTED_EDGE ( 'NONE', *, *, #8714, .T. ) ;
#8414 = LINE ( 'NONE', #4911, #13368 ) ;
#8416 = ADVANCED_FACE ( 'NONE', ( #2880, #10657, #12375 ), #10539, .F. ) ;
#8415 = LINE ( 'NONE', #1279, #12725 ) ;
#8417 = CIRCLE ( 'NONE', #4954, 2.649999999999985700 ) ;
#8418 = VECTOR ( 'NONE', #21685, 1000.000000000000000 ) ;
#8419 = DIRECTION ( 'NONE',  ( -1.000000000000000000, 1.408839003528726857E-14, 6.982962677686266711E-15 ) ) ;
#8420 = CIRCLE ( 'NONE', #14600, 0.2000000000000000944 ) ;
#8421 = ORIENTED_EDGE ( 'NONE', *, *, #3545, .T. ) ;
#8422 = LINE ( 'NONE', #5501, #6497 ) ;
#8423 = AXIS2_PLACEMENT_3D ( 'NONE', #10719, #14804, #8902 ) ;
#8424 = DIRECTION ( 'NONE',  ( -0.000000000000000000, -0.000000000000000000, 1.000000000000000000 ) ) ;
#8425 = DIRECTION ( 'NONE',  ( 1.000000000000000000, 0.000000000000000000, 0.000000000000000000 ) ) ;
#8426 = CARTESIAN_POINT ( 'NONE',  ( 65.00000000000004263, -52.79999999999959925, 65.00000000000018474 ) ) ;
#8427 = DIRECTION ( 'NONE',  ( -1.000000000000000000, -0.000000000000000000, 0.000000000000000000 ) ) ;
#8428 = DIRECTION ( 'NONE',  ( 1.000000000000000000, -6.640089860198304064E-16, -0.000000000000000000 ) ) ;
#8429 = CARTESIAN_POINT ( 'NONE',  ( -284.1320353020573179, 270.9755088701073191, 145.8700598572184504 ) ) ;
#8430 = EDGE_LOOP ( 'NONE', ( #3144, #6910, #17616, #22142 ) ) ;
#8431 = VERTEX_POINT ( 'NONE', #8702 ) ;
#8432 = DIRECTION ( 'NONE',  ( 6.753181414994864868E-15, 0.000000000000000000, -1.000000000000000000 ) ) ;
#8433 = CARTESIAN_POINT ( 'NONE',  ( -7.297096662748653293E-16, -8.716842316802402735, -7.700127545397317697 ) ) ;
#8434 = EDGE_LOOP ( 'NONE', ( #21020, #19042 ) ) ;
#8435 = PRODUCT_DEFINITION_SHAPE ( 'NONE', 'NONE',  #16109 ) ;
#8436 = CARTESIAN_POINT ( 'NONE',  ( 89.00000000000000000, -152.9999999999996874, 129.9038105676659711 ) ) ;
#8437 = EDGE_CURVE ( 'NONE', #11652, #9214, #14945, .T. ) ;
#8438 = AXIS2_PLACEMENT_3D ( 'NONE', #13273, #7677, #447 ) ;
#8439 = ADVANCED_FACE ( 'NONE', ( #5193 ), #19796, .F. ) ;
#8440 = AXIS2_PLACEMENT_3D ( 'NONE', #12886, #18612, #14438 ) ;
#8441 = EDGE_LOOP ( 'NONE', ( #4272, #19522 ) ) ;
#8442 = DIRECTION ( 'NONE',  ( -1.000000000000000000, 0.000000000000000000, 0.000000000000000000 ) ) ;
#8443 = CIRCLE ( 'NONE', #18074, 145.0000000000000284 ) ;
#8444 = EDGE_CURVE ( 'NONE', #11003, #1963, #23553, .T. ) ;
#8445 = DIRECTION ( 'NONE',  ( 0.000000000000000000, -3.495664435217746987E-15, 1.000000000000000000 ) ) ;
#8446 = ORIENTED_EDGE ( 'NONE', *, *, #13472, .T. ) ;
#8447 = EDGE_CURVE ( 'NONE', #9681, #8057, #9143, .T. ) ;
#8448 = CARTESIAN_POINT ( 'NONE',  ( -135.4687158836535161, -1075.321440059930637, -32.43450926607474827 ) ) ;
#8449 = VECTOR ( 'NONE', #815, 1000.000000000000000 ) ;
#8450 = ORIENTED_EDGE ( 'NONE', *, *, #1340, .F. ) ;
#8451 = ADVANCED_FACE ( 'NONE', ( #957 ), #8338, .F. ) ;
#8452 = DIRECTION ( 'NONE',  ( 4.625929269271484928E-16, -3.469446951953613794E-15, -1.000000000000000000 ) ) ;
#8453 = EDGE_CURVE ( 'NONE', #22988, #18096, #23405, .T. ) ;
#8454 = DIRECTION ( 'NONE',  ( 1.000000000000000000, -0.000000000000000000, -0.000000000000000000 ) ) ;
#8455 = ORIENTED_EDGE ( 'NONE', *, *, #3241, .T. ) ;
#8456 = VERTEX_POINT ( 'NONE', #10902 ) ;
#8457 = CARTESIAN_POINT ( 'NONE',  ( 134.1263161626748968, 77.68610759098272922, -29.83733181946745816 ) ) ;
#8458 = CIRCLE ( 'NONE', #10000, 5.000000000000001776 ) ;
#8459 = CARTESIAN_POINT ( 'NONE',  ( 1.360585162435110629, -4.061296242128317857, -3.505054077164905024 ) ) ;
#8460 = VECTOR ( 'NONE', #1107, 1000.000000000000000 ) ;
#8461 = VECTOR ( 'NONE', #4900, 1000.000000000000000 ) ;
#8462 = DIRECTION ( 'NONE',  ( 1.350636282998972974E-14, 0.000000000000000000, -1.000000000000000000 ) ) ;
#8463 = CARTESIAN_POINT ( 'NONE',  ( 0.000000000000000000, 0.000000000000000000, -50.00000000000000000 ) ) ;
#8464 = VECTOR ( 'NONE', #16590, 1000.000000000000114 ) ;
#8465 = EDGE_LOOP ( 'NONE', ( #11140, #391 ) ) ;
#8466 = CARTESIAN_POINT ( 'NONE',  ( -285.2000000000007276, 75.00000000000100897, -90.00000000000000000 ) ) ;
#8467 =( NAMED_UNIT ( * ) PLANE_ANGLE_UNIT ( ) SI_UNIT ( $, .RADIAN. ) );
#8468 = APPLICATION_CONTEXT ( 'automotive_design' ) ;
#8469 = ORIENTED_EDGE ( 'NONE', *, *, #15968, .T. ) ;
#8470 = EDGE_LOOP ( 'NONE', ( #21110, #14880 ) ) ;
#8471 = FACE_OUTER_BOUND ( 'NONE', #2288, .T. ) ;
#8473 = AXIS2_PLACEMENT_3D ( 'NONE', #1255, #21418, #17449 ) ;
#8472 = AXIS2_PLACEMENT_3D ( 'NONE', #11546, #8255, #17075 ) ;
#8474 = VERTEX_POINT ( 'NONE', #12954 ) ;
#8475 = CIRCLE ( 'NONE', #5382, 0.2000000000000000944 ) ;
#8476 = CARTESIAN_POINT ( 'NONE',  ( 281.4928932188134354, -127.0000000000000568, -150.2000000000013245 ) ) ;
#8477 = VECTOR ( 'NONE', #17078, 1000.000000000000000 ) ;
#8478 = CARTESIAN_POINT ( 'NONE',  ( 2.500000000000002220, 2.357898499370434386, -3.469446951953614189E-15 ) ) ;
#8479 = VECTOR ( 'NONE', #14927, 1000.000000000000000 ) ;
#8480 = VECTOR ( 'NONE', #19870, 1000.000000000000000 ) ;
#8481 = ORIENTED_EDGE ( 'NONE', *, *, #3534, .F. ) ;
#8482 = EDGE_CURVE ( 'NONE', #6820, #5659, #18226, .T. ) ;
#8483 = CARTESIAN_POINT ( 'NONE',  ( 90.00000000000000000, -149.9999999999996874, 129.9038105676659711 ) ) ;
#8484 = FACE_OUTER_BOUND ( 'NONE', #10415, .T. ) ;
#8485 = EDGE_CURVE ( 'NONE', #15233, #23406, #23657, .T. ) ;
#8486 = ORIENTED_EDGE ( 'NONE', *, *, #4099, .F. ) ;
#8487 = CARTESIAN_POINT ( 'NONE',  ( -44.99999999999997868, -56.79999999999937899, 140.0000000000001421 ) ) ;
#8488 =( NAMED_UNIT ( * ) SI_UNIT ( $, .STERADIAN. ) SOLID_ANGLE_UNIT ( ) );
#8489 = DIRECTION ( 'NONE',  ( 0.000000000000000000, -3.495664435217746987E-15, -1.000000000000000000 ) ) ;
#8490 = PLANE ( 'NONE',  #336 ) ;
#8491 = ORIENTED_EDGE ( 'NONE', *, *, #12765, .T. ) ;
#8492 = DIRECTION ( 'NONE',  ( -0.000000000000000000, -0.000000000000000000, 1.000000000000000000 ) ) ;
#8493 = COLOUR_RGB ( '',0.8941176470588234615, 0.8941176470588234615, 0.8941176470588234615 ) ;
#8494 = LINE ( 'NONE', #8361, #22712 ) ;
#8495 = AXIS2_PLACEMENT_3D ( 'NONE', #22492, #22246, #22612 ) ;
#8496 = AXIS2_PLACEMENT_3D ( 'NONE', #11028, #20404, #18350 ) ;
#8497 = AXIS2_PLACEMENT_3D ( 'NONE', #9507, #3926, #22283 ) ;
#8499 = VERTEX_POINT ( 'NONE', #14742 ) ;
#8498 = ORIENTED_EDGE ( 'NONE', *, *, #912, .T. ) ;
#8500 = DIRECTION ( 'NONE',  ( 2.832769448823989808E-16, -1.000000000000000000, 3.469446951953613794E-15 ) ) ;
#8501 = FACE_OUTER_BOUND ( 'NONE', #16141, .T. ) ;
#8502 = CARTESIAN_POINT ( 'NONE',  ( 4.000000000000000000, 0.000000000000000000, 0.000000000000000000 ) ) ;
#8503 = CYLINDRICAL_SURFACE ( 'NONE', #8844, 7.500000000000000000 ) ;
#8504 = DIRECTION ( 'NONE',  ( 0.000000000000000000, 0.000000000000000000, 1.000000000000000000 ) ) ;
#8505 = CARTESIAN_POINT ( 'NONE',  ( -284.1582675804706355, 270.9956429438695409, -145.8708543776411375 ) ) ;
#8506 = EDGE_LOOP ( 'NONE', ( #20531, #9827, #22800, #17026 ) ) ;
#8507 = CARTESIAN_POINT ( 'NONE',  ( -91.18044947428953151, 112.7436279071528702, -90.00000000000000000 ) ) ;
#8508 = ORIENTED_EDGE ( 'NONE', *, *, #8160, .T. ) ;
#8509 = FACE_BOUND ( 'NONE', #10636, .T. ) ;
#8510 = B_SPLINE_CURVE_WITH_KNOTS ( 'NONE', 3,
 ( #4163, #22402, #2359, #17097, #556, #9269 ),
 .UNSPECIFIED., .F., .F.,
 ( 4, 2, 4 ),
 ( 0.002365888236227995517, 0.003551327329835084114, 0.004736766423442172712 ),
 .UNSPECIFIED. ) ;
#8511 = DIRECTION ( 'NONE',  ( 0.000000000000000000, 0.000000000000000000, 1.000000000000000000 ) ) ;
#8512 = FILL_AREA_STYLE ('',( #21182 ) ) ;
#8513 = ITEM_DEFINED_TRANSFORMATION ( 'NONE', 'NONE', #3836,  #11210 ) ;
#8514 = ORIENTED_EDGE ( 'NONE', *, *, #20180, .T. ) ;
#8515 = VECTOR ( 'NONE', #13195, 1000.000000000000000 ) ;
#8516 = VECTOR ( 'NONE', #21049, 1000.000000000000000 ) ;
#8517 = DIRECTION ( 'NONE',  ( 1.000000000000000000, 0.000000000000000000, 0.000000000000000000 ) ) ;
#8518 = VERTEX_POINT ( 'NONE', #7118 ) ;
#8519 = CARTESIAN_POINT ( 'NONE',  ( 5.000000000000018652, 3.306546357697858171E-16, 2.699999999999997069 ) ) ;
#8520 = CYLINDRICAL_SURFACE ( 'NONE', #16798, 35.00000000000000000 ) ;
#8521 = VERTEX_POINT ( 'NONE', #9416 ) ;
#8522 = CARTESIAN_POINT ( 'NONE',  ( -281.3683070494395224, 268.4816199723481418, 150.1663417894422423 ) ) ;
#8523 = DIRECTION ( 'NONE',  ( 1.000000000000000000, 0.000000000000000000, 0.000000000000000000 ) ) ;
#8524 = CARTESIAN_POINT ( 'NONE',  ( 0.000000000000000000, 0.000000000000000000, 100.0000000000000000 ) ) ;
#8525 = CYLINDRICAL_SURFACE ( 'NONE', #21758, 2.649999999999971934 ) ;
#8526 = B_SPLINE_CURVE_WITH_KNOTS ( 'NONE', 3,
 ( #16849, #20950, #4295, #22512, #11698, #15654, #4407, #22983 ),
 .UNSPECIFIED., .F., .F.,
 ( 4, 2, 2, 4 ),
 ( 2.465131517390770070E-07, 0.001183067374689869946, 0.001774477805458935659, 0.002365888236228001588 ),
 .UNSPECIFIED. ) ;
#8527 = CARTESIAN_POINT ( 'NONE',  ( 25.00000000000001421, -37.41657386773940885, 169.9999999999999716 ) ) ;
#8528 = LINE ( 'NONE', #15899, #15038 ) ;
#8529 = CARTESIAN_POINT ( 'NONE',  ( -281.4928932188134922, 267.7999999999999545, -150.1999999999999602 ) ) ;
#8530 = ORIENTED_EDGE ( 'NONE', *, *, #11277, .F. ) ;
#8531 = SURFACE_SIDE_STYLE ('',( #13647 ) ) ;
#8532 = LINE ( 'NONE', #8641, #18051 ) ;
#8533 = CARTESIAN_POINT ( 'NONE',  ( -4.000000000000000000, 2.471528634177585282, -3.686887442155186712 ) ) ;
#8534 = EDGE_LOOP ( 'NONE', ( #3751, #12530 ) ) ;
#8535 = ORIENTED_EDGE ( 'NONE', *, *, #10655, .T. ) ;
#8536 = DIRECTION ( 'NONE',  ( 0.000000000000000000, 0.8660254037844391517, 0.4999999999999991673 ) ) ;
#8537 = DIRECTION ( 'NONE',  ( 1.000000000000000000, 0.000000000000000000, 0.000000000000000000 ) ) ;
#8539 = DIRECTION ( 'NONE',  ( -1.000000000000000000, 1.408839003528726857E-14, 6.982962677686266711E-15 ) ) ;
#8538 = PRODUCT_DEFINITION_SHAPE ( 'NONE', 'NONE',  #23856 ) ;
#8540 = DIRECTION ( 'NONE',  ( -1.000000000000000000, 0.000000000000000000, 0.000000000000000000 ) ) ;
#8541 = CARTESIAN_POINT ( 'NONE',  ( -283.4379565153279259, 271.7159870726003987, -145.6846668451111668 ) ) ;
#8542 = LINE ( 'NONE', #7177, #381 ) ;
#8543 = EDGE_LOOP ( 'NONE', ( #21925, #6923, #97, #11395 ) ) ;
#8544 = EDGE_CURVE ( 'NONE', #5300, #15719, #10716, .T. ) ;
#8545 = DIRECTION ( 'NONE',  ( -0.000000000000000000, -0.000000000000000000, -1.000000000000000000 ) ) ;
#8546 = CARTESIAN_POINT ( 'NONE',  ( 1.500000000000000000, 12.00000000000000000, 0.000000000000000000 ) ) ;
#8547 = ADVANCED_FACE ( 'NONE', ( #13200 ), #16088, .T. ) ;
#8548 = CARTESIAN_POINT ( 'NONE',  ( 45.24999999999996447, 100.0000000000000000, 150.2000000000009550 ) ) ;
#8549 = EDGE_CURVE ( 'NONE', #7103, #17283, #1913, .T. ) ;
#8550 = ORIENTED_EDGE ( 'NONE', *, *, #22469, .T. ) ;
#8551 = DIRECTION ( 'NONE',  ( 0.000000000000000000, -0.000000000000000000, 1.000000000000000000 ) ) ;
#8552 = DIRECTION ( 'NONE',  ( 0.000000000000000000, 0.000000000000000000, 1.000000000000000000 ) ) ;
#8553 = FACE_OUTER_BOUND ( 'NONE', #18562, .T. ) ;
#8554 = CARTESIAN_POINT ( 'NONE',  ( 15.25452100747948769, -1019.874440032434222, -145.0000000000001421 ) ) ;
#8555 = LINE ( 'NONE', #19760, #19224 ) ;
#8556 = EDGE_CURVE ( 'NONE', #22764, #11081, #9176, .T. ) ;
#8557 = CARTESIAN_POINT ( 'NONE',  ( 145.0000000000000284, 0.000000000000000000, 90.00000000000000000 ) ) ;
#8558 = CARTESIAN_POINT ( 'NONE',  ( -283.9159870726005579, 271.2379565153279373, 145.8082263737022686 ) ) ;
#8559 = ORIENTED_EDGE ( 'NONE', *, *, #18460, .T. ) ;
#8560 = ORIENTED_EDGE ( 'NONE', *, *, #12858, .T. ) ;
#8561 = CARTESIAN_POINT ( 'NONE',  ( -281.3673129565598288, 268.0906609804448522, -147.1854425596106637 ) ) ;
#8562 = CARTESIAN_POINT ( 'NONE',  ( -34.75000000000005684, 100.0000000000000000, -147.2000000000005571 ) ) ;
#8563 = ORIENTED_EDGE ( 'NONE', *, *, #8189, .T. ) ;
#8564 = CARTESIAN_POINT ( 'NONE',  ( -20.00000000000000000, 2.449293598294706513E-15, -100.0000000000000000 ) ) ;
#8565 = FACE_OUTER_BOUND ( 'NONE', #21396, .T. ) ;
#8566 = VERTEX_POINT ( 'NONE', #8954 ) ;
#8567 = FACE_OUTER_BOUND ( 'NONE', #18944, .T. ) ;
#8568 = LINE ( 'NONE', #9040, #1045 ) ;
#8569 = ORIENTED_EDGE ( 'NONE', *, *, #10441, .F. ) ;
#8570 = CARTESIAN_POINT ( 'NONE',  ( -134.7157571289271516, -1076.659463591458007, -31.25700618919322693 ) ) ;
#8571 = ORIENTED_EDGE ( 'NONE', *, *, #10506, .T. ) ;
#8572 = DIRECTION ( 'NONE',  ( 0.000000000000000000, 0.000000000000000000, -1.000000000000000000 ) ) ;
#8573 = PLANE ( 'NONE',  #22105 ) ;
#8574 = VERTEX_POINT ( 'NONE', #7362 ) ;
#8575 = ORIENTED_EDGE ( 'NONE', *, *, #2373, .F. ) ;
#8576 = CARTESIAN_POINT ( 'NONE',  ( 133.4121500950862469, 78.90641005980357647, -27.75009929603928072 ) ) ;
#8577 = EDGE_CURVE ( 'NONE', #4130, #12774, #12844, .T. ) ;
#8578 = FACE_OUTER_BOUND ( 'NONE', #16444, .T. ) ;
#8579 = EDGE_CURVE ( 'NONE', #10559, #17768, #233, .T. ) ;
#8580 = CARTESIAN_POINT ( 'NONE',  ( -4.419133455862249704, 6.108866147517435508, -7.026396753507433424 ) ) ;
#8581 = CYLINDRICAL_SURFACE ( 'NONE', #6264, 2.500000000000002220 ) ;
#8582 = EDGE_CURVE ( 'NONE', #17506, #1487, #10654, .T. ) ;
#8583 = ORIENTED_EDGE ( 'NONE', *, *, #22580, .T. ) ;
#8584 = CARTESIAN_POINT ( 'NONE',  ( -100.0000000000000000, 249.9999999999999716, 125.0000000000000284 ) ) ;
#8585 = ADVANCED_FACE ( 'NONE', ( #17027 ), #19045, .T. ) ;
#8586 = ORIENTED_EDGE ( 'NONE', *, *, #6019, .F. ) ;
#8587 = EDGE_CURVE ( 'NONE', #1686, #963, #1790, .T. ) ;
#8588 = VECTOR ( 'NONE', #13658, 1000.000000000000000 ) ;
#8589 = ORIENTED_EDGE ( 'NONE', *, *, #313, .T. ) ;
#8590 = DIRECTION ( 'NONE',  ( -1.000000000000000000, -3.736327486719275871E-16, -0.000000000000000000 ) ) ;
#8591 = ORIENTED_EDGE ( 'NONE', *, *, #18170, .F. ) ;
#8592 = CARTESIAN_POINT ( 'NONE',  ( 5.335963852943280017, 6.035591050531201596, -7.593821156097048330 ) ) ;
#8593 = ORIENTED_EDGE ( 'NONE', *, *, #6926, .T. ) ;
#8594 = CARTESIAN_POINT ( 'NONE',  ( -136.9304241666585824, -1072.629629052829841, 30.80845853161013892 ) ) ;
#8595 = LINE ( 'NONE', #10297, #16768 ) ;
#8596 = ORIENTED_EDGE ( 'NONE', *, *, #16136, .T. ) ;
#8597 = FACE_OUTER_BOUND ( 'NONE', #9188, .T. ) ;
#8598 = CARTESIAN_POINT ( 'NONE',  ( -280.3113419039146947, 269.8873946496626104, 145.7095819834011650 ) ) ;
#8599 = DIRECTION ( 'NONE',  ( -1.000000000000000000, 0.000000000000000000, -0.000000000000000000 ) ) ;
#8600 = CIRCLE ( 'NONE', #23627, 6.500000000000000888 ) ;
#8601 = APPLICATION_CONTEXT ( 'automotive_design' ) ;
#8602 = DIRECTION ( 'NONE',  ( 0.000000000000000000, 0.000000000000000000, 1.000000000000000000 ) ) ;
#8603 = CARTESIAN_POINT ( 'NONE',  ( 45.00000000000004974, -56.79999999999967031, 50.00000000000019895 ) ) ;
#8604 = ORIENTED_EDGE ( 'NONE', *, *, #59, .F. ) ;
#8605 = FACE_OUTER_BOUND ( 'NONE', #16623, .T. ) ;
#8606 =( LENGTH_UNIT ( ) NAMED_UNIT ( * ) SI_UNIT ( .MILLI., .METRE. ) );
#8608 = ORIENTED_EDGE ( 'NONE', *, *, #12694, .T. ) ;
#8607 = ORIENTED_EDGE ( 'NONE', *, *, #5439, .T. ) ;
#8609 = DIRECTION ( 'NONE',  ( 1.000000000000000000, 0.000000000000000000, 0.000000000000000000 ) ) ;
#8610 = EDGE_CURVE ( 'NONE', #4025, #12563, #7724, .T. ) ;
#8611 = EDGE_CURVE ( 'NONE', #20731, #8622, #16870, .T. ) ;
#8612 = CARTESIAN_POINT ( 'NONE',  ( 7.500000000000000000, 3.948247735265829395, -7.349893093595813554 ) ) ;
#8613 = CARTESIAN_POINT ( 'NONE',  ( 2.500000000000000000, 1.768423874527822459, -1.021000000000002794 ) ) ;
#8614 = EDGE_CURVE ( 'NONE', #14837, #11842, #13308, .T. ) ;
#8615 = CARTESIAN_POINT ( 'NONE',  ( 0.000000000000000000, -1.178949249685213863, 2.042000000000001148 ) ) ;
#8616 = PLANE ( 'NONE',  #7309 ) ;
#8617 = CARTESIAN_POINT ( 'NONE',  ( -282.1697000000000912, 268.0840560642353125, -146.3684665762323789 ) ) ;
#8618 = AXIS2_PLACEMENT_3D ( 'NONE', #6422, #11667, #9710 ) ;
#8619 = ORIENTED_EDGE ( 'NONE', *, *, #4184, .F. ) ;
#8620 = AXIS2_PLACEMENT_3D ( 'NONE', #18644, #13529, #16994 ) ;
#8621 = CARTESIAN_POINT ( 'NONE',  ( 0.000000000000000000, 2.357898499370432166, -2.385244779468109755E-15 ) ) ;
#8622 = VERTEX_POINT ( 'NONE', #20614 ) ;
#8623 = LINE ( 'NONE', #22008, #10005 ) ;
#8624 = DIRECTION ( 'NONE',  ( -1.000000000000000000, -0.000000000000000000, -0.000000000000000000 ) ) ;
#8625 = EDGE_LOOP ( 'NONE', ( #21321, #6812 ) ) ;
#8626 = DIRECTION ( 'NONE',  ( 1.000000000000000000, 0.000000000000000000, 0.000000000000000000 ) ) ;
#8627 = ORIENTED_EDGE ( 'NONE', *, *, #9935, .T. ) ;
#8628 = DIRECTION ( 'NONE',  ( 1.000000000000000000, 0.000000000000000000, -0.000000000000000000 ) ) ;
#8629 = DIRECTION ( 'NONE',  ( 0.000000000000000000, 0.000000000000000000, 1.000000000000000000 ) ) ;
#8630 = ORIENTED_EDGE ( 'NONE', *, *, #23531, .F. ) ;
#8631 = CARTESIAN_POINT ( 'NONE',  ( -281.4928932188135491, 267.7999999999999545, 150.1999999999999886 ) ) ;
#8632 = CARTESIAN_POINT ( 'NONE',  ( 1.500000000000000000, 0.000000000000000000, 150.0000000000000284 ) ) ;
#8633 = CIRCLE ( 'NONE', #7090, 7.499999999999998224 ) ;
#8634 = B_SPLINE_SURFACE_WITH_KNOTS ( 'NONE', 1, 3, ( 
 ( #18744, #17079, #20565, #15402, #6212, #13619, #16723, #7651, #9365, #15049 ),
 ( #4016, #2706, #1124, #4642, #8505, #4870, #8259, #13847, #23096, #8372 ),
 ( #2570, #22967, #10316, #21175, #15880, #12055, #15635, #23332, #4745, #15747 ),
 ( #13975, #8617, #23215, #2808, #12274, #6800, #3046, #14190, #15525, #22850 ) ),
 .UNSPECIFIED., .F., .F., .F.,
 ( 2, 1, 1, 2 ),
 ( 4, 2, 2, 2, 4 ),
 ( -0.01000000000000000021, 0.000000000000000000, 1.000000000000000000, 1.010099999999999998 ),
 ( 0.000000000000000000, 0.2500000000000000000, 0.5000000000000000000, 0.7500000000000000000, 1.000000000000000000 ),
 .UNSPECIFIED. ) ;
#8635 = VECTOR ( 'NONE', #15182, 1000.000000000000000 ) ;
#8636 = DIRECTION ( 'NONE',  ( -1.000000000000000000, 0.000000000000000000, 0.000000000000000000 ) ) ;
#8637 = CARTESIAN_POINT ( 'NONE',  ( 45.00000000000002132, -59.79999999999933635, 195.0000000000002558 ) ) ;
#8638 = DIRECTION ( 'NONE',  ( -1.000000000000000000, 0.000000000000000000, 0.000000000000000000 ) ) ;
#8639 = ORIENTED_EDGE ( 'NONE', *, *, #11142, .F. ) ;
#8640 = EDGE_CURVE ( 'NONE', #19464, #17109, #15106, .T. ) ;
#8641 = CARTESIAN_POINT ( 'NONE',  ( 235.0000000000000284, -490.0000000000001137, -60.00000000000000000 ) ) ;
#8642 = CARTESIAN_POINT ( 'NONE',  ( -285.2000000000011255, -29.99999999999898037, -102.3500000000000227 ) ) ;
#8643 = ORIENTED_EDGE ( 'NONE', *, *, #22012, .F. ) ;
#8644 = ORIENTED_EDGE ( 'NONE', *, *, #23781, .T. ) ;
#8645 = ADVANCED_FACE ( 'NONE', ( #11483, #7834 ), #9670, .T. ) ;
#8646 = CARTESIAN_POINT ( 'NONE',  ( 281.4928932188134354, 267.8000000000000114, -147.1999999999999318 ) ) ;
#8647 = CARTESIAN_POINT ( 'NONE',  ( -44.99999999999995026, -56.79999999999969873, 50.00000000000019895 ) ) ;
#8648 =( REPRESENTATION_RELATIONSHIP ('NONE','NONE', #10127, #22995 ) REPRESENTATION_RELATIONSHIP_WITH_TRANSFORMATION ( #2184 )SHAPE_REPRESENTATION_RELATIONSHIP( ) );
#8649 = CARTESIAN_POINT ( 'NONE',  ( -281.0927021017107563, 269.6958543268121957, 145.4976310729378213 ) ) ;
#8650 = MECHANICAL_DESIGN_GEOMETRIC_PRESENTATION_REPRESENTATION (  '', ( #545 ), #20991 ) ;
#8651 = VECTOR ( 'NONE', #13868, 1000.000000000000000 ) ;
#8652 = CARTESIAN_POINT ( 'NONE',  ( 4.000000000000003553, -2.309401076758513138, -3.504271511726786859 ) ) ;
#8653 = CARTESIAN_POINT ( 'NONE',  ( -283.9107452280325106, 271.2314821058793086, -145.8083875057488683 ) ) ;
#8654 = VERTEX_POINT ( 'NONE', #15219 ) ;
#8655 = DIRECTION ( 'NONE',  ( 0.000000000000000000, -1.000000000000000000, 0.000000000000000000 ) ) ;
#8656 = VERTEX_POINT ( 'NONE', #22550 ) ;
#8657 = FACE_OUTER_BOUND ( 'NONE', #21948, .T. ) ;
#8658 = DIRECTION ( 'NONE',  ( -0.000000000000000000, -0.000000000000000000, 1.000000000000000000 ) ) ;
#8659 = DIRECTION ( 'NONE',  ( 1.000000000000000000, 0.000000000000000000, 0.000000000000000000 ) ) ;
#8660 = EDGE_LOOP ( 'NONE', ( #1945, #5773, #7935, #14750 ) ) ;
#8661 = DIRECTION ( 'NONE',  ( 1.000000000000000000, 0.000000000000000000, 0.000000000000000000 ) ) ;
#8662 = CYLINDRICAL_SURFACE ( 'NONE', #9966, 2.649999999999971934 ) ;
#8663 = CARTESIAN_POINT ( 'NONE',  ( 312.2000000000013529, -132.2000000000000455, 146.4928932188134638 ) ) ;
#8664 = LINE ( 'NONE', #21918, #23291 ) ;
#8665 = CARTESIAN_POINT ( 'NONE',  ( 7.703011046602857601E-15, -132.2000000000000455, 146.4928932188134638 ) ) ;
#8666 = CARTESIAN_POINT ( 'NONE',  ( -285.2000000000013529, -89.99999999999897682, 24.33333333333333215 ) ) ;
#8667 = EDGE_CURVE ( 'NONE', #23173, #3845, #17625, .T. ) ;
#8668 = DIRECTION ( 'NONE',  ( -1.000000000000000000, -0.000000000000000000, -0.000000000000000000 ) ) ;
#8669 = AXIS2_PLACEMENT_3D ( 'NONE', #664, #6098, #15298 ) ;
#8670 = ORIENTED_EDGE ( 'NONE', *, *, #8752, .T. ) ;
#8671 = VECTOR ( 'NONE', #21185, 1000.000000000000114 ) ;
#8672 = ORIENTED_EDGE ( 'NONE', *, *, #22375, .F. ) ;
#8673 = DIRECTION ( 'NONE',  ( 1.000000000000000000, 0.000000000000000000, 0.000000000000000000 ) ) ;
#8674 = CARTESIAN_POINT ( 'NONE',  ( 281.0571734979477014, 268.7755403010747273, 146.9771302778488860 ) ) ;
#8675 = VERTEX_POINT ( 'NONE', #9778 ) ;
#8676 = VECTOR ( 'NONE', #18579, 1000.000000000000000 ) ;
#8677 = VECTOR ( 'NONE', #8129, 1000.000000000000000 ) ;
#8678 = EDGE_CURVE ( 'NONE', #20782, #9681, #1057, .T. ) ;
#8679 = DIRECTION ( 'NONE',  ( 0.000000000000000000, 0.000000000000000000, 1.000000000000000000 ) ) ;
#8680 = CARTESIAN_POINT ( 'NONE',  ( 1.411581201560190495E-15, 4.862606272033091592, -3.745885042887436622 ) ) ;
#8681 = ADVANCED_FACE ( 'NONE', ( #22802, #6380 ), #827, .T. ) ;
#8682 = ORIENTED_EDGE ( 'NONE', *, *, #415, .T. ) ;
#8683 = LINE ( 'NONE', #12351, #2523 ) ;
#8684 = CARTESIAN_POINT ( 'NONE',  ( -32.35000000000004405, 90.00000000000001421, 3.000000000000000000 ) ) ;
#8685 = EDGE_LOOP ( 'NONE', ( #17224, #14171 ) ) ;
#8686 = CARTESIAN_POINT ( 'NONE',  ( -135.7895026000616667, -1074.740959209979792, -27.49999999999351985 ) ) ;
#8687 = ADVANCED_FACE ( 'NONE', ( #8087 ), #15335, .F. ) ;
#8688 = AXIS2_PLACEMENT_3D ( 'NONE', #7206, #8808, #1768 ) ;
#8689 = VERTEX_POINT ( 'NONE', #6267 ) ;
#8690 = SURFACE_STYLE_FILL_AREA ( #22148 ) ;
#8691 = CARTESIAN_POINT ( 'NONE',  ( -4.000000000000004441, 2.309401076758496263, -3.504269196027523847 ) ) ;
#8692 = VERTEX_POINT ( 'NONE', #22672 ) ;
#8693 = ORIENTED_EDGE ( 'NONE', *, *, #4109, .T. ) ;
#8694 = CARTESIAN_POINT ( 'NONE',  ( 133.6263423143007572, 78.54310546248434832, -28.00764941310470135 ) ) ;
#8695 = VECTOR ( 'NONE', #3726, 1000.000000000000114 ) ;
#8696 = CARTESIAN_POINT ( 'NONE',  ( -277.2000000000014097, -89.99999999999900524, 24.33333333333333215 ) ) ;
#8697 = CLOSED_SHELL ( 'NONE', ( #22289, #1948, #16698, #16922, #13730, #14798, #21718, #1303, #6273, #7179, #12342, #13602, #17137, #3406, #19439, #21747, #10137, #21373, #16925, #9635, #14154, #11552, #3048, #458, #2727, #212, #351, #5200, #8845, #21709, #7486, #861, #16541, #10180, #3671, #6027, #1798, #146, #21400, #15637, #13415, #15215, #12634, #6270, #1030, #13428, #19497, #10644, #5834, #18380, #14024, #12503, #5760, #13892, #2040, #10234, #18742, #1130, #23270, #752, #5043, #13970, #13788, #18330, #21288, #481, #23532, #19028, #14047, #10542, #10643, #7128, #9520, #23671, #6021, #2063, #15608, #2302, #5850, #117, #5491, #20397, #2197, #20654, #270, #10915, #11504, #2959, #22015, #6193, #8158, #6539, #20351, #18982, #19866, #21977, #23187, #20492, #19805, #20559, #8268, #8905, #8407, #3002, #23730, #15545, #14014, #14900, #3280, #4066, #15420, #5529 ) ) ;
#8698 = CARTESIAN_POINT ( 'NONE',  ( 279.9999999999999432, 267.7999999999999545, 146.4928932188134922 ) ) ;
#8699 = CARTESIAN_POINT ( 'NONE',  ( -5.088535779737005882, 5.722386535631696525, -7.491772860716161553 ) ) ;
#8700 = DIRECTION ( 'NONE',  ( 4.183096374613631247E-18, 1.000000000000000000, 0.000000000000000000 ) ) ;
#8701 = ORIENTED_EDGE ( 'NONE', *, *, #183, .T. ) ;
#8702 = CARTESIAN_POINT ( 'NONE',  ( -72.64999999999996305, -112.6666666666667140, 0.000000000000000000 ) ) ;
#8703 = AXIS2_PLACEMENT_3D ( 'NONE', #17389, #18934, #7958 ) ;
#8704 = EDGE_LOOP ( 'NONE', ( #19337, #13827, #3744, #1489 ) ) ;
#8705 = ADVANCED_FACE ( 'NONE', ( #15470 ), #12276, .F. ) ;
#8706 = EDGE_CURVE ( 'NONE', #21291, #17822, #8391, .T. ) ;
#8707 = COLOUR_RGB ( '',1.000000000000000000, 0.9490196078431372140, 0.9098039215686274384 ) ;
#8708 = DIRECTION ( 'NONE',  ( 0.000000000000000000, 1.000000000000000000, 0.000000000000000000 ) ) ;
#8709 = AXIS2_PLACEMENT_3D ( 'NONE', #2761, #22913, #19660 ) ;
#8710 = LINE ( 'NONE', #10662, #21848 ) ;
#8711 = ORIENTED_EDGE ( 'NONE', *, *, #431, .F. ) ;
#8712 = CARTESIAN_POINT ( 'NONE',  ( 7.777900015783946408, 4.169681370001526055, -7.928862157988300297 ) ) ;
#8713 = EDGE_CURVE ( 'NONE', #23038, #22261, #4805, .T. ) ;
#8714 = EDGE_CURVE ( 'NONE', #22000, #22474, #10731, .T. ) ;
#8715 = ORIENTED_EDGE ( 'NONE', *, *, #8970, .T. ) ;
#8716 = VECTOR ( 'NONE', #7542, 1000.000000000000000 ) ;
#8717 = DIRECTION ( 'NONE',  ( -1.000000000000000000, 0.000000000000000000, 0.000000000000000000 ) ) ;
#8718 = EDGE_LOOP ( 'NONE', ( #10530, #19645, #10578, #10680 ) ) ;
#8719 = EDGE_CURVE ( 'NONE', #23365, #17297, #1805, .T. ) ;
#8720 = PRODUCT_RELATED_PRODUCT_CATEGORY ( 'part', '', ( #20003 ) ) ;
#8721 = DIRECTION ( 'NONE',  ( 0.000000000000000000, 0.000000000000000000, -1.000000000000000000 ) ) ;
#8722 = CARTESIAN_POINT ( 'NONE',  ( -281.0571594757294065, 268.7755899421580921, 146.9771650631953719 ) ) ;
#8723 = EDGE_CURVE ( 'NONE', #1031, #6562, #7999, .T. ) ;
#8724 = PLANE ( 'NONE',  #16514 ) ;
#8725 = VECTOR ( 'NONE', #10582, 1000.000000000000000 ) ;
#8726 = DIRECTION ( 'NONE',  ( 0.000000000000000000, -3.469446951953614583E-15, -1.000000000000000000 ) ) ;
#8727 = CARTESIAN_POINT ( 'NONE',  ( -128.5330911521621431, -1074.345258785412625, 30.00000000000641620 ) ) ;
#8728 = ORIENTED_EDGE ( 'NONE', *, *, #9758, .T. ) ;
#8729 = DIRECTION ( 'NONE',  ( 0.000000000000000000, 0.000000000000000000, 1.000000000000000000 ) ) ;
#8730 = SURFACE_STYLE_USAGE ( .BOTH. , #14069 ) ;
#8731 = PRODUCT_DEFINITION_SHAPE ( 'NONE', 'NONE',  #23829 ) ;
#8733 = EDGE_LOOP ( 'NONE', ( #2254, #9465 ) ) ;
#8732 = EDGE_LOOP ( 'NONE', ( #5276, #13813, #23184, #21223 ) ) ;
#8734 = DIRECTION ( 'NONE',  ( 2.832769448823989808E-16, -1.000000000000000000, 3.469446951953613794E-15 ) ) ;
#8735 = LINE ( 'NONE', #9212, #15055 ) ;
#8736 = AXIS2_PLACEMENT_3D ( 'NONE', #9092, #20076, #3397 ) ;
#8737 = DIRECTION ( 'NONE',  ( -1.000000000000000000, -0.000000000000000000, -0.000000000000000000 ) ) ;
#8738 = DIRECTION ( 'NONE',  ( 0.000000000000000000, 0.000000000000000000, -1.000000000000000000 ) ) ;
#8739 = CARTESIAN_POINT ( 'NONE',  ( 144.8060344827587187, -7.497491405670202447, -90.00000000000000000 ) ) ;
#8740 = EDGE_CURVE ( 'NONE', #1295, #21317, #16045, .T. ) ;
#8741 = ORIENTED_EDGE ( 'NONE', *, *, #2161, .T. ) ;
#8742 = EDGE_CURVE ( 'NONE', #15596, #14669, #14193, .T. ) ;
#8743 = CARTESIAN_POINT ( 'NONE',  ( -40.00000000000000000, 100.0000000000000000, 150.2000000000009550 ) ) ;
#8744 = EDGE_LOOP ( 'NONE', ( #547, #15983, #16105, #15606 ) ) ;
#8745 = ADVANCED_FACE ( 'NONE', ( #10260 ), #1053, .T. ) ;
#8746 = DIRECTION ( 'NONE',  ( -1.000000000000000000, 0.000000000000000000, 0.000000000000000000 ) ) ;
#8747 = CARTESIAN_POINT ( 'NONE',  ( -285.2000000000008981, 35.00000000000100897, 105.0000000000000000 ) ) ;
#8748 = CONTEXT_DEPENDENT_SHAPE_REPRESENTATION ( #12400, #19102 ) ;
#8749 = ORIENTED_EDGE ( 'NONE', *, *, #16864, .F. ) ;
#8750 = ORIENTED_EDGE ( 'NONE', *, *, #84, .T. ) ;
#8751 = CARTESIAN_POINT ( 'NONE',  ( -129.3180659214438890, 85.45079184243574844, -30.32849798811265885 ) ) ;
#8752 = EDGE_CURVE ( 'NONE', #13397, #16062, #1293, .T. ) ;
#8753 = CARTESIAN_POINT ( 'NONE',  ( -45.00000000000000000, 250.0000000000000000, 5.249999999999956479 ) ) ;
#8754 = ADVANCED_FACE ( 'NONE', ( #17486 ), #18783, .F. ) ;
#8755 = ORIENTED_EDGE ( 'NONE', *, *, #6830, .T. ) ;
#8756 = VECTOR ( 'NONE', #8590, 1000.000000000000000 ) ;
#8757 = ADVANCED_FACE ( 'NONE', ( #11985 ), #12675, .F. ) ;
#8758 = CARTESIAN_POINT ( 'NONE',  ( -281.4301685943534039, 268.1431883566699526, 150.1999999999999602 ) ) ;
#8759 = ORIENTED_EDGE ( 'NONE', *, *, #7567, .F. ) ;
#8760 = CARTESIAN_POINT ( 'NONE',  ( 133.6912351773691228, 78.43256762916516323, 31.88926668738024972 ) ) ;
#8761 = DIRECTION ( 'NONE',  ( 0.000000000000000000, 2.618450529776326854E-15, 1.000000000000000000 ) ) ;
#8762 = CARTESIAN_POINT ( 'NONE',  ( 158.0000000000000284, 3.114171532854473382E-14, -56.99999999999973710 ) ) ;
#8763 = CYLINDRICAL_SURFACE ( 'NONE', #22693, 21.02499999999999503 ) ;
#8764 = CARTESIAN_POINT ( 'NONE',  ( -20.00000000000000000, 2.449293598294706513E-15, -150.0000000000000000 ) ) ;
#8765 = CARTESIAN_POINT ( 'NONE',  ( 40.00000000000000000, 100.0000000000000000, -145.0000000000000284 ) ) ;
#8766 = ORIENTED_EDGE ( 'NONE', *, *, #11219, .T. ) ;
#8767 = CARTESIAN_POINT ( 'NONE',  ( 0.000000000000000000, 0.000000000000000000, -25.03750572909317285 ) ) ;
#8768 = CARTESIAN_POINT ( 'NONE',  ( 0.1750025118121568690, 4.719839900820621104, -3.469254087858248070 ) ) ;
#8769 = VECTOR ( 'NONE', #22313, 1000.000000000000000 ) ;
#8770 = ORIENTED_EDGE ( 'NONE', *, *, #16941, .F. ) ;
#8771 = CARTESIAN_POINT ( 'NONE',  ( 99.99999999999987210, -127.0000000000000568, 150.2000000000014381 ) ) ;
#8772 = CYLINDRICAL_SURFACE ( 'NONE', #17579, 2.500000000000002220 ) ;
#8773 = AXIS2_PLACEMENT_3D ( 'NONE', #17393, #4338, #13921 ) ;
#8774 = CARTESIAN_POINT ( 'NONE',  ( -280.0000000000000568, 272.9999999999999432, 145.0000000000000284 ) ) ;
#8775 = DIRECTION ( 'NONE',  ( 1.000000000000000000, 0.000000000000000000, 0.000000000000000000 ) ) ;
#8776 = DIRECTION ( 'NONE',  ( 1.000000000000000000, -1.408839003528726857E-14, -6.982962677686266711E-15 ) ) ;
#8777 = ORIENTED_EDGE ( 'NONE', *, *, #15086, .F. ) ;
#8778 = DIRECTION ( 'NONE',  ( 1.000000000000000000, 0.000000000000000000, 0.000000000000000000 ) ) ;
#8779 = ORIENTED_EDGE ( 'NONE', *, *, #6493, .F. ) ;
#8780 = DIRECTION ( 'NONE',  ( -1.000000000000000000, -0.000000000000000000, -0.000000000000000000 ) ) ;
#8781 = CARTESIAN_POINT ( 'NONE',  ( 45.00000000000000000, 269.9999999999999432, 0.000000000000000000 ) ) ;
#8782 = EDGE_CURVE ( 'NONE', #22261, #12527, #10320, .T. ) ;
#8783 = EDGE_CURVE ( 'NONE', #3110, #9858, #23788, .T. ) ;
#8784 = FILL_AREA_STYLE_COLOUR ( '', #7868 ) ;
#8785 = ORIENTED_EDGE ( 'NONE', *, *, #17170, .T. ) ;
#8786 = VECTOR ( 'NONE', #5635, 1000.000000000000000 ) ;
#8787 = CARTESIAN_POINT ( 'NONE',  ( -281.4928932188135491, -127.0000000000000568, 152.4000000000014268 ) ) ;
#8788 = CARTESIAN_POINT ( 'NONE',  ( 155.0000000000000284, -500.0000000000000000, 30.00000000000001421 ) ) ;
#8789 = EDGE_CURVE ( 'NONE', #9214, #11652, #13429, .T. ) ;
#8790 = CARTESIAN_POINT ( 'NONE',  ( 155.0000000000000568, -801.0618695410399823, 30.00000000000648015 ) ) ;
#8791 = DIRECTION ( 'NONE',  ( 1.000000000000000000, 0.000000000000000000, 0.000000000000000000 ) ) ;
#8793 = AXIS2_PLACEMENT_3D ( 'NONE', #10202, #15884, #14195 ) ;
#8792 = DIRECTION ( 'NONE',  ( 1.000000000000000000, 0.000000000000000000, 0.000000000000000000 ) ) ;
#8794 = CYLINDRICAL_SURFACE ( 'NONE', #4590, 4.250000000000000000 ) ;
#8795 = VECTOR ( 'NONE', #20249, 1000.000000000000000 ) ;
#8796 = CARTESIAN_POINT ( 'NONE',  ( 25.00000000000000355, 1.636246173744694277, 145.0000119999999697 ) ) ;
#8797 = EDGE_LOOP ( 'NONE', ( #4434, #800 ) ) ;
#8798 = EDGE_LOOP ( 'NONE', ( #20347, #4489, #13008, #10684 ) ) ;
#8799 = CARTESIAN_POINT ( 'NONE',  ( -280.0000000000000000, 270.0000000000000000, -144.9999999999999716 ) ) ;
#8800 = CARTESIAN_POINT ( 'NONE',  ( 146.0000000000002274, -210.0000000000003411, -29.99999999999356604 ) ) ;
#8801 = EDGE_LOOP ( 'NONE', ( #2185, #20140, #16234, #14079 ) ) ;
#8802 = FACE_BOUND ( 'NONE', #5929, .T. ) ;
#8803 = AXIS2_PLACEMENT_3D ( 'NONE', #12895, #16128, #20202 ) ;
#8804 = EDGE_LOOP ( 'NONE', ( #4456, #6614, #22048, #8560 ) ) ;
#8805 = FACE_OUTER_BOUND ( 'NONE', #2556, .T. ) ;
#8806 = DIRECTION ( 'NONE',  ( 0.000000000000000000, 0.000000000000000000, 1.000000000000000000 ) ) ;
#8807 = VERTEX_POINT ( 'NONE', #17598 ) ;
#8808 = DIRECTION ( 'NONE',  ( 0.000000000000000000, -3.495664435217746987E-15, 1.000000000000000000 ) ) ;
#8809 = VECTOR ( 'NONE', #18192, 1000.000000000000000 ) ;
#8810 = ORIENTED_EDGE ( 'NONE', *, *, #17016, .F. ) ;
#8811 = DIRECTION ( 'NONE',  ( 0.000000000000000000, 0.000000000000000000, 1.000000000000000000 ) ) ;
#8812 = CARTESIAN_POINT ( 'NONE',  ( -4.154094228333456762, 2.398367420968013253, -3.721909803043220055 ) ) ;
#8813 = ORIENTED_EDGE ( 'NONE', *, *, #9013, .F. ) ;
#8814 = ORIENTED_EDGE ( 'NONE', *, *, #19198, .F. ) ;
#8815 = CARTESIAN_POINT ( 'NONE',  ( -59.99999999999996447, -138.3994082814338071, -3.599999999999746070 ) ) ;
#8816 = EDGE_CURVE ( 'NONE', #3965, #2180, #23272, .T. ) ;
#8817 = DIRECTION ( 'NONE',  ( 1.000000000000000000, 0.000000000000000000, 6.123233995736766036E-17 ) ) ;
#8818 = CARTESIAN_POINT ( 'NONE',  ( -285.2000000000008981, 30.00000000000101963, -105.0000000000000142 ) ) ;
#8819 = CARTESIAN_POINT ( 'NONE',  ( 0.000000000000000000, 0.000000000000000000, -9.226681596905677907 ) ) ;
#8820 = FACE_OUTER_BOUND ( 'NONE', #484, .T. ) ;
#8821 = ORIENTED_EDGE ( 'NONE', *, *, #12306, .F. ) ;
#8822 = AXIS2_PLACEMENT_3D ( 'NONE', #3208, #22696, #10620 ) ;
#8823 = FACE_OUTER_BOUND ( 'NONE', #21564, .T. ) ;
#8824 = VECTOR ( 'NONE', #18976, 1000.000000000000000 ) ;
#8825 = AXIS2_PLACEMENT_3D ( 'NONE', #8141, #8247, #19444 ) ;
#8826 = VERTEX_POINT ( 'NONE', #23265 ) ;
#8827 = AXIS2_PLACEMENT_3D ( 'NONE', #10364, #10244, #21450 ) ;
#8828 = FACE_OUTER_BOUND ( 'NONE', #1607, .T. ) ;
#8829 = DIRECTION ( 'NONE',  ( -0.7071067811865364705, 8.659560562355067211E-17, -0.7071067811865584529 ) ) ;
#8830 = EDGE_LOOP ( 'NONE', ( #4777, #15202, #20661, #2331 ) ) ;
#8831 = CARTESIAN_POINT ( 'NONE',  ( 2.500000000000000000, 1.178949249685212974, -2.042000000000001148 ) ) ;
#8832 = VERTEX_POINT ( 'NONE', #6738 ) ;
#8833 = B_SPLINE_SURFACE_WITH_KNOTS ( 'NONE', 1, 3, ( 
 ( #21244, #15587, #14026, #14141, #21471, #6385, #4573, #21822, #14265, #5066 ),
 ( #18424, #18097, #23534, #10882, #12472, #5518, #12934, #9154, #12583, #1550 ),
 ( #1886, #16398, #9039, #23401, #23749, #3474, #16511, #5657, #6859, #5416 ),
 ( #7203, #1657, #8938, #21607, #7340, #19774, #6992, #18311, #14721, #18208 ) ),
 .UNSPECIFIED., .F., .F., .F.,
 ( 2, 1, 1, 2 ),
 ( 4, 2, 2, 2, 4 ),
 ( -0.01000000000000000021, 0.000000000000000000, 1.000000000000000000, 1.010099999999999998 ),
 ( 0.000000000000000000, 0.2500000000000000000, 0.5000000000000000000, 0.7500000000000000000, 1.000000000000000000 ),
 .UNSPECIFIED. ) ;
#8834 = AXIS2_PLACEMENT_3D ( 'NONE', #11819, #8175, #9986 ) ;
#8835 = TOROIDAL_SURFACE ( 'NONE', #5741, 2.700000000000000622, 0.2000000000000000111 ) ;
#8836 = FACE_OUTER_BOUND ( 'NONE', #8873, .T. ) ;
#8837 = AXIS2_PLACEMENT_3D ( 'NONE', #3287, #16344, #7041 ) ;
#8838 = CIRCLE ( 'NONE', #19229, 7.500000000000003553 ) ;
#8839 = EDGE_LOOP ( 'NONE', ( #14071, #8953, #10562, #17132 ) ) ;
#8840 = CIRCLE ( 'NONE', #10008, 2.499999999999998668 ) ;
#8841 = EDGE_CURVE ( 'NONE', #21770, #22523, #14960, .T. ) ;
#8842 = DIRECTION ( 'NONE',  ( 0.000000000000000000, 0.000000000000000000, 1.000000000000000000 ) ) ;
#8843 = EDGE_CURVE ( 'NONE', #12980, #9344, #5278, .T. ) ;
#8844 = AXIS2_PLACEMENT_3D ( 'NONE', #17907, #21295, #15877 ) ;
#8845 = ADVANCED_FACE ( 'NONE', ( #23740, #8509, #12820 ), #21926, .T. ) ;
#8846 = DIRECTION ( 'NONE',  ( -1.000000000000000000, -0.000000000000000000, -0.000000000000000000 ) ) ;
#8847 = SHAPE_REPRESENTATION ( 'head pulley', ( #11210 ), #17342 ) ;
#8848 = DIRECTION ( 'NONE',  ( -0.000000000000000000, -0.000000000000000000, 1.000000000000000000 ) ) ;
#8849 = DIRECTION ( 'NONE',  ( 0.000000000000000000, -1.000000000000000000, 9.256405414277014607E-16 ) ) ;
#8850 = EDGE_LOOP ( 'NONE', ( #17006, #868, #12144 ) ) ;
#8851 = DIRECTION ( 'NONE',  ( -1.000000000000000000, 0.000000000000000000, 0.000000000000000000 ) ) ;
#8852 = EDGE_CURVE ( 'NONE', #7786, #1506, #12671, .T. ) ;
#8854 = ORIENTED_EDGE ( 'NONE', *, *, #14172, .T. ) ;
#8853 = ORIENTED_EDGE ( 'NONE', *, *, #19222, .T. ) ;
#8855 =( GEOMETRIC_REPRESENTATION_CONTEXT ( 3 ) GLOBAL_UNCERTAINTY_ASSIGNED_CONTEXT ( ( #2685 ) ) GLOBAL_UNIT_ASSIGNED_CONTEXT ( ( #414, #19335, #6784 ) ) REPRESENTATION_CONTEXT ( 'NONE', 'WORKASPACE' ) );
#8856 = UNCERTAINTY_MEASURE_WITH_UNIT (LENGTH_MEASURE( 1.000000000000000082E-05 ), #11883, 'distance_accuracy_value', 'NONE');
#8858 = AXIS2_PLACEMENT_3D ( 'NONE', #15993, #18257, #1482 ) ;
#8857 = DIRECTION ( 'NONE',  ( 1.000000000000000000, 0.000000000000000000, 0.000000000000000000 ) ) ;
#8860 = VECTOR ( 'NONE', #3740, 1000.000000000000000 ) ;
#8859 = STYLED_ITEM ( 'NONE', ( #12184 ), #17647 ) ;
#8861 = DIRECTION ( 'NONE',  ( 0.000000000000000000, 0.000000000000000000, -1.000000000000000000 ) ) ;
#8862 = CARTESIAN_POINT ( 'NONE',  ( 281.4928932188134354, -132.2000000000000455, -150.2000000000013245 ) ) ;
#8863 = VECTOR ( 'NONE', #11578, 1000.000000000000114 ) ;
#8864 = VECTOR ( 'NONE', #19009, 1000.000000000000000 ) ;
#8865 = AXIS2_PLACEMENT_3D ( 'NONE', #18873, #7649, #15160 ) ;
#8866 = COLOUR_RGB ( '',1.000000000000000000, 0.9490196078431372140, 0.9098039215686274384 ) ;
#8867 = CIRCLE ( 'NONE', #5771, 35.00000000000000000 ) ;
#8868 = DIRECTION ( 'NONE',  ( -1.000000000000000000, 0.000000000000000000, 0.000000000000000000 ) ) ;
#8869 = DIRECTION ( 'NONE',  ( 0.000000000000000000, 1.000000000000000000, 0.000000000000000000 ) ) ;
#8870 = ADVANCED_FACE ( 'NONE', ( #18200 ), #18417, .F. ) ;
#8871 = ORIENTED_EDGE ( 'NONE', *, *, #6495, .T. ) ;
#8872 = FACE_OUTER_BOUND ( 'NONE', #23160, .T. ) ;
#8873 = EDGE_LOOP ( 'NONE', ( #7761, #18869, #20724, #20914 ) ) ;
#8874 = CARTESIAN_POINT ( 'NONE',  ( -37.30746418436648071, -137.9031948627975908, 90.00000000000000000 ) ) ;
#8875 = CARTESIAN_POINT ( 'NONE',  ( 1.567478505476135000E-15, 4.618802153517012954, -3.504269196027527844 ) ) ;
#8876 = ITEM_DEFINED_TRANSFORMATION ( 'NONE', 'NONE', #14671,  #11210 ) ;
#8877 = ORIENTED_EDGE ( 'NONE', *, *, #1336, .F. ) ;
#8878 = ORIENTED_EDGE ( 'NONE', *, *, #3076, .T. ) ;
#8879 = CARTESIAN_POINT ( 'NONE',  ( 0.2500000000000002220, 0.000000000000000000, 2.081668171172168513E-14 ) ) ;
#8881 = VECTOR ( 'NONE', #19243, 1000.000000000000000 ) ;
#8880 = AXIS2_PLACEMENT_3D ( 'NONE', #7895, #4633, #13366 ) ;
#8882 = ORIENTED_EDGE ( 'NONE', *, *, #20222, .T. ) ;
#8883 = PRESENTATION_LAYER_ASSIGNMENT (  '', '', ( #14675 ) ) ;
#8884 = CIRCLE ( 'NONE', #13929, 2.649999999999985700 ) ;
#8885 = CARTESIAN_POINT ( 'NONE',  ( 133.8109447024529004, 78.22816056888504477, 31.65640384616916947 ) ) ;
#8886 = AXIS2_PLACEMENT_3D ( 'NONE', #16788, #3969, #22691 ) ;
#8887 = AXIS2_PLACEMENT_3D ( 'NONE', #3215, #10627, #828 ) ;
#8888 = CARTESIAN_POINT ( 'NONE',  ( -285.2000000000006708, 90.00000000000102318, -32.35000000000004405 ) ) ;
#8889 = PLANE ( 'NONE',  #15229 ) ;
#8890 = CARTESIAN_POINT ( 'NONE',  ( 2.500000000000000000, 2.357898499370432166, -2.385244779468109755E-15 ) ) ;
#8891 = DIRECTION ( 'NONE',  ( -1.000000000000000000, 0.000000000000000000, 0.000000000000000000 ) ) ;
#8892 = EDGE_CURVE ( 'NONE', #8313, #10742, #19546, .T. ) ;
#8893 = CIRCLE ( 'NONE', #6566, 2.649999999999985700 ) ;
#8894 = EDGE_CURVE ( 'NONE', #12339, #539, #21815, .T. ) ;
#8895 = ORIENTED_EDGE ( 'NONE', *, *, #2658, .F. ) ;
#8896 = ADVANCED_FACE ( 'NONE', ( #13043 ), #16503, .F. ) ;
#8897 = CARTESIAN_POINT ( 'NONE',  ( 2.500000000000000000, 2.357898499370431722, -2.818925648462311528E-15 ) ) ;
#8898 = CARTESIAN_POINT ( 'NONE',  ( -2.712762565639006418, 3.052587955997511759, -3.430618716626627318 ) ) ;
#8899 = VERTEX_POINT ( 'NONE', #16288 ) ;
#8900 = EDGE_CURVE ( 'NONE', #20731, #17846, #5679, .T. ) ;
#8901 = DIRECTION ( 'NONE',  ( 0.000000000000000000, -1.000000000000000000, 6.123233995736766036E-17 ) ) ;
#8902 = DIRECTION ( 'NONE',  ( 0.000000000000000000, 0.000000000000000000, 1.000000000000000000 ) ) ;
#8903 = PRODUCT_RELATED_PRODUCT_CATEGORY ( 'part', '', ( #5359 ) ) ;
#8904 = ORIENTED_EDGE ( 'NONE', *, *, #6369, .F. ) ;
#8905 = ADVANCED_FACE ( 'NONE', ( #10744 ), #5161, .F. ) ;
#8906 = MECHANICAL_DESIGN_GEOMETRIC_PRESENTATION_REPRESENTATION (  '', ( #13111 ), #16932 ) ;
#8907 = AXIS2_PLACEMENT_3D ( 'NONE', #2136, #2503, #9896 ) ;
#8908 = LINE ( 'NONE', #10601, #16769 ) ;
#8909 = AXIS2_PLACEMENT_3D ( 'NONE', #7560, #14951, #16745 ) ;
#8910 = CARTESIAN_POINT ( 'NONE',  ( 155.0000000000000284, -500.0000000000000000, 60.00000000000002132 ) ) ;
#8911 = CARTESIAN_POINT ( 'NONE',  ( 7.499999999999997335, 34.18698582794336005, 100.0000000000000000 ) ) ;
#8912 = ORIENTED_EDGE ( 'NONE', *, *, #3122, .T. ) ;
#8913 = FACE_BOUND ( 'NONE', #4171, .T. ) ;
#8914 = ORIENTED_EDGE ( 'NONE', *, *, #10570, .F. ) ;
#8915 = FACE_OUTER_BOUND ( 'NONE', #17534, .T. ) ;
#8916 = CARTESIAN_POINT ( 'NONE',  ( 93.00000000000000000, -149.9999999999996874, 129.9038105676659711 ) ) ;
#8917 =( NAMED_UNIT ( * ) SI_UNIT ( $, .STERADIAN. ) SOLID_ANGLE_UNIT ( ) );
#8918 = VERTEX_POINT ( 'NONE', #3683 ) ;
#8919 = CARTESIAN_POINT ( 'NONE',  ( -6.293430271071534854, 5.026740376715094882, -0.4524126574264483169 ) ) ;
#8920 = DIRECTION ( 'NONE',  ( 1.000000000000000000, 0.000000000000000000, 0.000000000000000000 ) ) ;
#8921 = FACE_OUTER_BOUND ( 'NONE', #11520, .T. ) ;
#8922 = FACE_BOUND ( 'NONE', #5978, .T. ) ;
#8923 = APPLICATION_CONTEXT ( 'automotive_design' ) ;
#8924 = DIRECTION ( 'NONE',  ( 0.000000000000000000, -1.177509268541832635E-16, 1.000000000000000000 ) ) ;
#8925 = DIRECTION ( 'NONE',  ( -1.000000000000000000, -2.775557561562891351E-17, 0.000000000000000000 ) ) ;
#8926 = CARTESIAN_POINT ( 'NONE',  ( 16.52066876451829103, 18.83467029480909360, 145.0000119999999697 ) ) ;
#8927 = ORIENTED_EDGE ( 'NONE', *, *, #4696, .T. ) ;
#8928 = EDGE_LOOP ( 'NONE', ( #13313, #14377, #919, #8038 ) ) ;
#8929 = CARTESIAN_POINT ( 'NONE',  ( 0.000000000000000000, 0.000000000000000000, -150.0000000000000000 ) ) ;
#8930 = DIRECTION ( 'NONE',  ( 1.350636282998972974E-14, 0.000000000000000000, -1.000000000000000000 ) ) ;
#8931 = ORIENTED_EDGE ( 'NONE', *, *, #7230, .T. ) ;
#8932 = FACE_OUTER_BOUND ( 'NONE', #12438, .T. ) ;
#8933 = DIRECTION ( 'NONE',  ( 0.000000000000000000, 0.000000000000000000, -1.000000000000000000 ) ) ;
#8934 = ADVANCED_FACE ( 'NONE', ( #18544 ), #3466, .F. ) ;
#8935 = EDGE_CURVE ( 'NONE', #21483, #11736, #19947, .T. ) ;
#8936 = ADVANCED_FACE ( 'NONE', ( #1540 ), #23630, .F. ) ;
#8937 = ORIENTED_EDGE ( 'NONE', *, *, #13795, .T. ) ;
#8938 = CARTESIAN_POINT ( 'NONE',  ( 280.2488155364687827, 269.9132285165672442, 145.5679143846943475 ) ) ;
#8939 = FACE_OUTER_BOUND ( 'NONE', #21756, .T. ) ;
#8940 = EDGE_LOOP ( 'NONE', ( #12135, #17491, #11708, #2332 ) ) ;
#8941 = DIRECTION ( 'NONE',  ( 0.000000000000000000, 0.000000000000000000, 1.000000000000000000 ) ) ;
#8942 = ORIENTED_EDGE ( 'NONE', *, *, #14743, .T. ) ;
#8943 = CARTESIAN_POINT ( 'NONE',  ( 29.55500000000002458, 0.000000000000000000, -6.938893903907228378E-15 ) ) ;
#8944 = CARTESIAN_POINT ( 'NONE',  ( 0.000000000000000000, 0.000000000000000000, 169.9999999999999716 ) ) ;
#8945 = CARTESIAN_POINT ( 'NONE',  ( 2.500000000000000000, 2.357898499370432166, -2.385244779468109755E-15 ) ) ;
#8946 = VERTEX_POINT ( 'NONE', #10876 ) ;
#8947 = ORIENTED_EDGE ( 'NONE', *, *, #11829, .T. ) ;
#8948 = CARTESIAN_POINT ( 'NONE',  ( 285.0646579186752660, 269.1610889986682196, -146.2440776823444537 ) ) ;
#8949 = CARTESIAN_POINT ( 'NONE',  ( 40.00000000000000000, 100.0000000000000000, -160.2000000000005855 ) ) ;
#8950 = CARTESIAN_POINT ( 'NONE',  ( -127.0272233253969318, 88.82062435172005621, -28.00764941310471201 ) ) ;
#8951 = CARTESIAN_POINT ( 'NONE',  ( -0.9763930676156993282, 8.096533237421580154, -7.213065638943424673 ) ) ;
#8952 = LINE ( 'NONE', #9307, #11728 ) ;
#8953 = ORIENTED_EDGE ( 'NONE', *, *, #594, .T. ) ;
#8954 = CARTESIAN_POINT ( 'NONE',  ( -135.7895026000616667, -1074.740959209979792, -27.49999999999351985 ) ) ;
#8955 =( NAMED_UNIT ( * ) SI_UNIT ( $, .STERADIAN. ) SOLID_ANGLE_UNIT ( ) );
#8956 = DIRECTION ( 'NONE',  ( -1.000000000000000000, 1.408839003528726857E-14, 6.982962677686266711E-15 ) ) ;
#8957 = LINE ( 'NONE', #21496, #17612 ) ;
#8958 = ORIENTED_EDGE ( 'NONE', *, *, #14505, .T. ) ;
#8959 = DIRECTION ( 'NONE',  ( 0.000000000000000000, -1.287488025362403787E-15, -1.000000000000000000 ) ) ;
#8960 = ORIENTED_EDGE ( 'NONE', *, *, #8614, .F. ) ;
#8961 = DIRECTION ( 'NONE',  ( 1.000000000000000000, 0.000000000000000000, 0.000000000000000000 ) ) ;
#8962 = ORIENTED_EDGE ( 'NONE', *, *, #20230, .T. ) ;
#8963 = DIRECTION ( 'NONE',  ( -0.000000000000000000, -0.000000000000000000, 1.000000000000000000 ) ) ;
#8964 = FACE_OUTER_BOUND ( 'NONE', #22981, .T. ) ;
#8965 = CARTESIAN_POINT ( 'NONE',  ( -281.4928932188134354, 35.00000000000022737, -113.4834095219707848 ) ) ;
#8966 = CARTESIAN_POINT ( 'NONE',  ( -0.5974722283283655511, 8.315303285985683246, -0.7026937717022859742 ) ) ;
#8967 = CARTESIAN_POINT ( 'NONE',  ( 110.0000000000000000, -74.99999999999998579, 3.000000000000000000 ) ) ;
#8968 = ORIENTED_EDGE ( 'NONE', *, *, #1443, .T. ) ;
#8969 = LINE ( 'NONE', #14310, #21935 ) ;
#8970 = EDGE_CURVE ( 'NONE', #17386, #13236, #12298, .T. ) ;
#8972 = ORIENTED_EDGE ( 'NONE', *, *, #12603, .F. ) ;
#8971 = ORIENTED_EDGE ( 'NONE', *, *, #10950, .T. ) ;
#8973 = DIRECTION ( 'NONE',  ( 6.123233995736766036E-17, -1.000000000000000000, 0.000000000000000000 ) ) ;
#8974 = DIRECTION ( 'NONE',  ( 1.350636282998972974E-14, 0.000000000000000000, -1.000000000000000000 ) ) ;
#8975 = CYLINDRICAL_SURFACE ( 'NONE', #9968, 35.00000000000000000 ) ;
#8976 = EDGE_LOOP ( 'NONE', ( #19175, #9567 ) ) ;
#8977 = CIRCLE ( 'NONE', #10928, 2.649999999999971934 ) ;
#8978 = EDGE_CURVE ( 'NONE', #17822, #21291, #16490, .T. ) ;
#8979 = CARTESIAN_POINT ( 'NONE',  ( -285.2000000000014666, -127.0000000000000568, 0.000000000000000000 ) ) ;
#8980 = EDGE_CURVE ( 'NONE', #11081, #1322, #23048, .T. ) ;
#8981 = CARTESIAN_POINT ( 'NONE',  ( 0.000000000000000000, -1000.000000000000000, -150.0000000000000000 ) ) ;
#8982 = VERTEX_POINT ( 'NONE', #18770 ) ;
#8983 = LINE ( 'NONE', #19839, #10024 ) ;
#8984 = CARTESIAN_POINT ( 'NONE',  ( 2.548804901056335857E-15, 4.736522675502163437, -3.681124513963624612 ) ) ;
#8985 = ADVANCED_FACE ( 'NONE', ( #17106 ), #22519, .F. ) ;
#8986 = VERTEX_POINT ( 'NONE', #15076 ) ;
#8987 = SHAPE_REPRESENTATION ( 'socket head cap screw_iso_ISO 4762 M5 x 30 - 22N', ( #11210 ), #18837 ) ;
#8988 = VECTOR ( 'NONE', #476, 1000.000000000000000 ) ;
#8989 = VERTEX_POINT ( 'NONE', #2234 ) ;
#8990 = DIRECTION ( 'NONE',  ( 0.000000000000000000, -1.000000000000000000, 1.287488025362403787E-15 ) ) ;
#8991 = ORIENTED_EDGE ( 'NONE', *, *, #7055, .F. ) ;
#8992 = CARTESIAN_POINT ( 'NONE',  ( 155.0000000000000284, -500.0000000000000000, -27.49999999999996803 ) ) ;
#8993 = CARTESIAN_POINT ( 'NONE',  ( 132.9250442248334139, 79.72427207779767855, 32.50000000000646594 ) ) ;
#8994 = CARTESIAN_POINT ( 'NONE',  ( 4.211399257449709665, -2.459727064652517114, -3.751161691472417736 ) ) ;
#8995 = CARTESIAN_POINT ( 'NONE',  ( -40.00000000000000000, 100.0000000000000000, -125.0000000000000000 ) ) ;
#8996 = CARTESIAN_POINT ( 'NONE',  ( 91.18044947429038416, -112.7436279071521881, 90.00000000000000000 ) ) ;
#8997 = LINE ( 'NONE', #1839, #20031 ) ;
#8998 = ORIENTED_EDGE ( 'NONE', *, *, #22708, .F. ) ;
#8999 = FILL_AREA_STYLE ('',( #23361 ) ) ;
#9000 = CYLINDRICAL_SURFACE ( 'NONE', #2220, 5.000000000000000888 ) ;
#9001 = CARTESIAN_POINT ( 'NONE',  ( 7.914984360234579519, -3.818534719232097974, -7.907701344400643428 ) ) ;
#9002 = AXIS2_PLACEMENT_3D ( 'NONE', #10342, #2829, #13992 ) ;
#9003 = VERTEX_POINT ( 'NONE', #6240 ) ;
#9004 = CARTESIAN_POINT ( 'NONE',  ( 280.1255802622536635, 269.9854425596107035, -145.2906609804447555 ) ) ;
#9005 = DIRECTION ( 'NONE',  ( 0.000000000000000000, 0.000000000000000000, -1.000000000000000000 ) ) ;
#9006 = DIRECTION ( 'NONE',  ( 0.000000000000000000, -1.000000000000000000, 0.000000000000000000 ) ) ;
#9007 = DIRECTION ( 'NONE',  ( -1.000000000000000000, 0.000000000000000000, 0.000000000000000000 ) ) ;
#9008 = CARTESIAN_POINT ( 'NONE',  ( 280.7774350431395760, 271.3570580646226631, -148.7968359015655437 ) ) ;
#9009 = EDGE_CURVE ( 'NONE', #15698, #23312, #16997, .T. ) ;
#9010 = ORIENTED_EDGE ( 'NONE', *, *, #5550, .T. ) ;
#9012 = VECTOR ( 'NONE', #17086, 1000.000000000000000 ) ;
#9011 = DIRECTION ( 'NONE',  ( -0.000000000000000000, -0.000000000000000000, 1.000000000000000000 ) ) ;
#9013 = EDGE_CURVE ( 'NONE', #18629, #14819, #10749, .T. ) ;
#9014 = ORIENTED_EDGE ( 'NONE', *, *, #23444, .T. ) ;
#9015 = DIRECTION ( 'NONE',  ( -0.000000000000000000, -0.000000000000000000, 1.000000000000000000 ) ) ;
#9016 = LINE ( 'NONE', #14361, #1484 ) ;
#9017 = CIRCLE ( 'NONE', #13678, 24.69999999999999929 ) ;
#9018 = ORIENTED_EDGE ( 'NONE', *, *, #11275, .F. ) ;
#9019 = ADVANCED_FACE ( 'NONE', ( #20961 ), #7682, .F. ) ;
#9020 = CARTESIAN_POINT ( 'NONE',  ( 7.500000000000000000, -4.330127018922199866, -10.00000000000000000 ) ) ;
#9021 = DIRECTION ( 'NONE',  ( 0.000000000000000000, -3.495664435217746987E-15, 1.000000000000000000 ) ) ;
#9022 = PLANE ( 'NONE',  #18269 ) ;
#9023 = CARTESIAN_POINT ( 'NONE',  ( 52.00000000000000711, -56.79999999999999005, 5.199999999999971756 ) ) ;
#9024 = ADVANCED_FACE ( 'NONE', ( #2482, #14949, #22776, #562, #16857, #9870, #11827, #675, #5990 ), #11455, .F. ) ;
#9025 = DIRECTION ( 'NONE',  ( -3.736327486719275871E-16, 1.000000000000000000, 0.000000000000000000 ) ) ;
#9026 = LINE ( 'NONE', #18197, #17480 ) ;
#9027 = ORIENTED_EDGE ( 'NONE', *, *, #19170, .T. ) ;
#9028 = ORIENTED_EDGE ( 'NONE', *, *, #14228, .T. ) ;
#9029 = ADVANCED_BREP_SHAPE_REPRESENTATION ( '', ( #12378, #11210 ), #1924 ) ;
#9030 = DIRECTION ( 'NONE',  ( -0.9510565162951510887, -0.3090169943749553894, 0.000000000000000000 ) ) ;
#9031 = FACE_OUTER_BOUND ( 'NONE', #7723, .T. ) ;
#9032 = ORIENTED_EDGE ( 'NONE', *, *, #10465, .F. ) ;
#9033 = AXIS2_PLACEMENT_3D ( 'NONE', #9166, #16524, #16412 ) ;
#9034 = PRODUCT_DEFINITION_SHAPE ( 'NONE', 'NONE',  #12164 ) ;
#9035 = LINE ( 'NONE', #18202, #10851 ) ;
#9037 = AXIS2_PLACEMENT_3D ( 'NONE', #7080, #19993, #10618 ) ;
#9036 = CARTESIAN_POINT ( 'NONE',  ( 2.325424218458714165, -7.317669739337183898, -7.030005583191490715 ) ) ;
#9038 = ORIENTED_EDGE ( 'NONE', *, *, #20885, .F. ) ;
#9039 = CARTESIAN_POINT ( 'NONE',  ( 280.2488155364687827, 269.9427398886703031, 145.5758453455904373 ) ) ;
#9040 = CARTESIAN_POINT ( 'NONE',  ( 50.00000000000000000, 5.109226446042757607E-16, -4.171999999999999709 ) ) ;
#9041 = ORIENTED_EDGE ( 'NONE', *, *, #17411, .T. ) ;
#9042 = EDGE_CURVE ( 'NONE', #21146, #11458, #2114, .T. ) ;
#9043 = FACE_OUTER_BOUND ( 'NONE', #7236, .T. ) ;
#9044 = DIRECTION ( 'NONE',  ( 1.000000000000000000, 0.000000000000000000, 0.000000000000000000 ) ) ;
#9045 = ORIENTED_EDGE ( 'NONE', *, *, #9179, .F. ) ;
#9046 = DIRECTION ( 'NONE',  ( -1.000000000000000000, 6.640089860198304064E-16, 0.000000000000000000 ) ) ;
#9047 = CARTESIAN_POINT ( 'NONE',  ( -135.7895026000614109, -1074.740959209980247, 32.50000000000646594 ) ) ;
#9048 = CARTESIAN_POINT ( 'NONE',  ( -4.000000000000000000, 2.309401076758498483, -3.433295621305379353 ) ) ;
#9049 = ORIENTED_EDGE ( 'NONE', *, *, #17309, .T. ) ;
#9050 = ORIENTED_EDGE ( 'NONE', *, *, #20562, .T. ) ;
#9051 = CARTESIAN_POINT ( 'NONE',  ( 285.2299999999999045, 268.4847249064869743, -146.3684637172358123 ) ) ;
#9052 = CIRCLE ( 'NONE', #15214, 2.500000000000000888 ) ;
#9053 = DIRECTION ( 'NONE',  ( 1.000000000000000000, 0.000000000000000000, 6.123233995736766036E-17 ) ) ;
#9054 = CARTESIAN_POINT ( 'NONE',  ( -126.8176664439032919, 89.11954614941136299, -28.34359615383082343 ) ) ;
#9055 = AXIS2_PLACEMENT_3D ( 'NONE', #19478, #15429, #2935 ) ;
#9056 = EDGE_CURVE ( 'NONE', #9146, #5513, #19137, .T. ) ;
#9057 = EDGE_CURVE ( 'NONE', #10540, #2069, #20710, .T. ) ;
#9058 = CARTESIAN_POINT ( 'NONE',  ( -59.99999999999996447, 1.830696786719878692E-29, 3.000000000000000000 ) ) ;
#9059 = DIRECTION ( 'NONE',  ( -1.000000000000000000, 1.408839003528726857E-14, 6.982962677686266711E-15 ) ) ;
#9060 = VERTEX_POINT ( 'NONE', #4172 ) ;
#9061 = CARTESIAN_POINT ( 'NONE',  ( -21.69578997558839362, -12.52876685377503563, 145.0000119999999697 ) ) ;
#9062 = LINE ( 'NONE', #13078, #21038 ) ;
#9063 = DIRECTION ( 'NONE',  ( -1.000000000000000000, 0.000000000000000000, 0.000000000000000000 ) ) ;
#9064 = CIRCLE ( 'NONE', #8294, 5.249999999999949374 ) ;
#9065 = ORIENTED_EDGE ( 'NONE', *, *, #20321, .T. ) ;
#9066 = CARTESIAN_POINT ( 'NONE',  ( -100.0000000000000853, -127.0000000000000568, 152.4000000000014268 ) ) ;
#9067 = VECTOR ( 'NONE', #20272, 1000.000000000000000 ) ;
#9068 = AXIS2_PLACEMENT_3D ( 'NONE', #96, #19021, #2491 ) ;
#9069 = ORIENTED_EDGE ( 'NONE', *, *, #12569, .T. ) ;
#9070 = EDGE_CURVE ( 'NONE', #3139, #10051, #13278, .T. ) ;
#9071 = LINE ( 'NONE', #3261, #18675 ) ;
#9072 = CARTESIAN_POINT ( 'NONE',  ( -4.235886605889389145, -2.417314728048544303, -3.751161874094020909 ) ) ;
#9073 = ORIENTED_EDGE ( 'NONE', *, *, #12155, .T. ) ;
#9074 = LINE ( 'NONE', #5448, #22733 ) ;
#9075 = EDGE_CURVE ( 'NONE', #7205, #8322, #11586, .T. ) ;
#9076 = AXIS2_PLACEMENT_3D ( 'NONE', #11739, #13309, #19046 ) ;
#9077 = CARTESIAN_POINT ( 'NONE',  ( 21.69578997558838296, -1012.528766853774982, 145.0000119999999697 ) ) ;
#9078 = CARTESIAN_POINT ( 'NONE',  ( -52.99999999999997158, -62.00000000000001421, -3.122502256758252770E-14 ) ) ;
#9079 = CYLINDRICAL_SURFACE ( 'NONE', #3929, 2.649999999999999467 ) ;
#9080 = ADVANCED_FACE ( 'NONE', ( #20478 ), #323, .F. ) ;
#9081 = LINE ( 'NONE', #16440, #18099 ) ;
#9082 = ORIENTED_EDGE ( 'NONE', *, *, #3452, .T. ) ;
#9083 = LINE ( 'NONE', #6908, #17269 ) ;
#9084 = SURFACE_STYLE_USAGE ( .BOTH. , #38 ) ;
#9085 = AXIS2_PLACEMENT_3D ( 'NONE', #11810, #9736, #19123 ) ;
#9087 = ORIENTED_EDGE ( 'NONE', *, *, #1195, .F. ) ;
#9086 = ORIENTED_EDGE ( 'NONE', *, *, #10036, .F. ) ;
#9088 = DIRECTION ( 'NONE',  ( 1.221966984364620947E-29, 3.495664435217746987E-15, -1.000000000000000000 ) ) ;
#9089 = CARTESIAN_POINT ( 'NONE',  ( -44.99999999999995026, -52.79999999999968452, 102.3500000000002075 ) ) ;
#9090 = PLANE ( 'NONE',  #12687 ) ;
#9091 = VERTEX_POINT ( 'NONE', #2365 ) ;
#9092 = CARTESIAN_POINT ( 'NONE',  ( -40.00000000000000000, 100.0000000000000000, -145.0000000000000284 ) ) ;
#9093 = CIRCLE ( 'NONE', #5616, 2.041999999999999815 ) ;
#9094 = CYLINDRICAL_SURFACE ( 'NONE', #9165, 4.250000000000000000 ) ;
#9095 = ORIENTED_EDGE ( 'NONE', *, *, #6944, .T. ) ;
#9096 = CIRCLE ( 'NONE', #6005, 2.055000000000001492 ) ;
#9097 = FACE_OUTER_BOUND ( 'NONE', #15275, .T. ) ;
#9098 = CARTESIAN_POINT ( 'NONE',  ( -3.974344831685191280E-13, 4.796734841935104576, -3.721909803043223608 ) ) ;
#9099 = ITEM_DEFINED_TRANSFORMATION ( 'NONE', 'NONE', #21972,  #11210 ) ;
#9100 = EDGE_CURVE ( 'NONE', #23060, #2744, #11523, .T. ) ;
#9101 = ORIENTED_EDGE ( 'NONE', *, *, #11417, .F. ) ;
#9102 = CIRCLE ( 'NONE', #3291, 160.0000000000000000 ) ;
#9103 = ORIENTED_EDGE ( 'NONE', *, *, #2944, .F. ) ;
#9104 = CARTESIAN_POINT ( 'NONE',  ( 0.000000000000000000, -1.178949249685215417, 2.042000000000002036 ) ) ;
#9105 = ORIENTED_EDGE ( 'NONE', *, *, #15084, .T. ) ;
#9106 =( REPRESENTATION_RELATIONSHIP ('NONE','NONE', #10127, #4815 ) REPRESENTATION_RELATIONSHIP_WITH_TRANSFORMATION ( #12789 )SHAPE_REPRESENTATION_RELATIONSHIP( ) );
#9107 = CARTESIAN_POINT ( 'NONE',  ( 24.99999999999998224, -1000.000000000000000, -145.0000060000000417 ) ) ;
#9108 = CARTESIAN_POINT ( 'NONE',  ( 2.500000000000002220, 0.000000000000000000, 0.000000000000000000 ) ) ;
#9109 = ADVANCED_FACE ( 'NONE', ( #15309 ), #9506, .F. ) ;
#9110 = CARTESIAN_POINT ( 'NONE',  ( 4.211405965630455661, 2.460463115436283932, -3.751298928144577882 ) ) ;
#9111 = EDGE_CURVE ( 'NONE', #10145, #1663, #13876, .T. ) ;
#9112 = DIRECTION ( 'NONE',  ( -0.000000000000000000, -0.000000000000000000, 1.000000000000000000 ) ) ;
#9113 = CARTESIAN_POINT ( 'NONE',  ( 0.2500000000000002220, 0.000000000000000000, 0.000000000000000000 ) ) ;
#9114 = VECTOR ( 'NONE', #9843, 1000.000000000000000 ) ;
#9115 = SURFACE_STYLE_FILL_AREA ( #16826 ) ;
#9116 = ORIENTED_EDGE ( 'NONE', *, *, #15108, .F. ) ;
#9117 = DIRECTION ( 'NONE',  ( 1.000000000000000000, 0.000000000000000000, 0.000000000000000000 ) ) ;
#9118 = CARTESIAN_POINT ( 'NONE',  ( -7.500000000000000888, 3.639598441879742907, -0.7155132341745253921 ) ) ;
#9119 = DIRECTION ( 'NONE',  ( -1.000000000000000000, 0.000000000000000000, 0.000000000000000000 ) ) ;
#9120 = EDGE_CURVE ( 'NONE', #23021, #16805, #19736, .T. ) ;
#9121 = ORIENTED_EDGE ( 'NONE', *, *, #20620, .T. ) ;
#9122 = CARTESIAN_POINT ( 'NONE',  ( 280.4986342070537830, 269.7080393212557397, -146.1045205713627126 ) ) ;
#9123 = PLANE ( 'NONE',  #4170 ) ;
#9124 = CARTESIAN_POINT ( 'NONE',  ( -285.2000000000000455, 268.4807971656551331, 146.3684637452624884 ) ) ;
#9125 = CIRCLE ( 'NONE', #2950, 2.649999999999985700 ) ;
#9126 = DIRECTION ( 'NONE',  ( 0.000000000000000000, 0.000000000000000000, 1.000000000000000000 ) ) ;
#9127 = DIRECTION ( 'NONE',  ( 0.7071067811865416886, 0.000000000000000000, -0.7071067811865532349 ) ) ;
#9128 = CARTESIAN_POINT ( 'NONE',  ( 5.000000000000004441, 0.000000000000000000, 4.250000000000000000 ) ) ;
#9129 = ORIENTED_EDGE ( 'NONE', *, *, #10251, .T. ) ;
#9130 = DIRECTION ( 'NONE',  ( 0.000000000000000000, 0.000000000000000000, 1.000000000000000000 ) ) ;
#9131 = ORIENTED_EDGE ( 'NONE', *, *, #14512, .T. ) ;
#9132 = CARTESIAN_POINT ( 'NONE',  ( 4.000000000000000000, -2.309401076758514915, -3.433295621305383349 ) ) ;
#9133 = DIRECTION ( 'NONE',  ( 0.000000000000000000, 1.000000000000000000, -1.471414886128461471E-15 ) ) ;
#9134 = ORIENTED_EDGE ( 'NONE', *, *, #5322, .F. ) ;
#9135 = DIRECTION ( 'NONE',  ( 0.000000000000000000, 0.000000000000000000, 1.000000000000000000 ) ) ;
#9136 = CARTESIAN_POINT ( 'NONE',  ( 123.5476367174094179, -1093.600214943837500, -28.00764941310472977 ) ) ;
#9137 = ADVANCED_FACE ( 'NONE', ( #10227 ), #9178, .F. ) ;
#9138 = LINE ( 'NONE', #16492, #6518 ) ;
#9139 = CARTESIAN_POINT ( 'NONE',  ( 2.500000000000000000, -1.178949249685213863, 2.042000000000002924 ) ) ;
#9140 = ADVANCED_FACE ( 'NONE', ( #12081 ), #3377, .F. ) ;
#9141 = CARTESIAN_POINT ( 'NONE',  ( -282.2000000000012960, -74.99999999999899103, -90.00000000000000000 ) ) ;
#9142 = LINE ( 'NONE', #22046, #15793 ) ;
#9143 = CIRCLE ( 'NONE', #22617, 0.2500000000000002220 ) ;
#9144 = DIRECTION ( 'NONE',  ( -0.000000000000000000, -0.000000000000000000, -1.000000000000000000 ) ) ;
#9145 = ORIENTED_EDGE ( 'NONE', *, *, #10817, .T. ) ;
#9146 = VERTEX_POINT ( 'NONE', #14218 ) ;
#9147 = DIRECTION ( 'NONE',  ( 0.000000000000000000, 0.000000000000000000, 1.000000000000000000 ) ) ;
#9148 = AXIS2_PLACEMENT_3D ( 'NONE', #13433, #17030, #20747 ) ;
#9149 = CARTESIAN_POINT ( 'NONE',  ( -146.0000000000005116, -784.4690652294799520, -29.99999999999356604 ) ) ;
#9150 = ADVANCED_FACE ( 'NONE', ( #1015 ), #22880, .T. ) ;
#9151 = ORIENTED_EDGE ( 'NONE', *, *, #6248, .F. ) ;
#9152 = CARTESIAN_POINT ( 'NONE',  ( -282.2000000000000455, 267.7999999999999545, 145.0000000000000284 ) ) ;
#9153 = ORIENTED_EDGE ( 'NONE', *, *, #8285, .T. ) ;
#9154 = CARTESIAN_POINT ( 'NONE',  ( 281.2440776823444253, 269.1610889986682196, 150.0646579186752376 ) ) ;
#9155 = DIRECTION ( 'NONE',  ( -1.000000000000000000, 0.000000000000000000, 0.000000000000000000 ) ) ;
#9156 = EDGE_CURVE ( 'NONE', #4760, #14572, #8532, .T. ) ;
#9157 = VERTEX_POINT ( 'NONE', #23124 ) ;
#9158 = DIRECTION ( 'NONE',  ( -0.000000000000000000, 1.000000000000000000, -0.000000000000000000 ) ) ;
#9159 = CARTESIAN_POINT ( 'NONE',  ( -4.000000000000000000, 0.7924765000094600165, -0.05906175389889745803 ) ) ;
#9160 = AXIS2_PLACEMENT_3D ( 'NONE', #6016, #15578, #4450 ) ;
#9161 = DIRECTION ( 'NONE',  ( 0.000000000000000000, 0.000000000000000000, 1.000000000000000000 ) ) ;
#9162 = ORIENTED_EDGE ( 'NONE', *, *, #19795, .F. ) ;
#9163 = DIRECTION ( 'NONE',  ( 0.000000000000000000, -0.5000000000000013323, -0.8660254037844380415 ) ) ;
#9164 = CARTESIAN_POINT ( 'NONE',  ( -136.5237489982504826, -1073.391313005787879, 28.00660068667239955 ) ) ;
#9165 = AXIS2_PLACEMENT_3D ( 'NONE', #7395, #11173, #10819 ) ;
#9166 = CARTESIAN_POINT ( 'NONE',  ( 155.0000000000000284, -500.0000000000000000, -29.99999999999997158 ) ) ;
#9167 = VECTOR ( 'NONE', #23256, 1000.000000000000000 ) ;
#9168 = EDGE_LOOP ( 'NONE', ( #17567, #6787 ) ) ;
#9169 = ORIENTED_EDGE ( 'NONE', *, *, #17022, .F. ) ;
#9170 = FACE_OUTER_BOUND ( 'NONE', #3146, .T. ) ;
#9171 = APPLICATION_PROTOCOL_DEFINITION ( 'draft international standard', 'automotive_design', 1998, #11093 ) ;
#9172 = CARTESIAN_POINT ( 'NONE',  ( -127.8082730365391058, 87.69306101368243844, -32.49999999999352696 ) ) ;
#9173 = LINE ( 'NONE', #475, #3427 ) ;
#9174 = DIRECTION ( 'NONE',  ( -1.000000000000000000, 0.000000000000000000, 0.000000000000000000 ) ) ;
#9175 = ORIENTED_EDGE ( 'NONE', *, *, #20096, .T. ) ;
#9176 = LINE ( 'NONE', #20379, #3350 ) ;
#9177 = EDGE_CURVE ( 'NONE', #16083, #18758, #14213, .T. ) ;
#9178 = CONICAL_SURFACE ( 'NONE', #2610, 2.500000000000000888, 0.9599310885968785900 ) ;
#9179 = EDGE_CURVE ( 'NONE', #21004, #20797, #17637, .T. ) ;
#9180 = EDGE_CURVE ( 'NONE', #14990, #23782, #1077, .T. ) ;
#9181 = CIRCLE ( 'NONE', #18411, 2.500000000000000444 ) ;
#9182 = VECTOR ( 'NONE', #16251, 1000.000000000000000 ) ;
#9183 = UNCERTAINTY_MEASURE_WITH_UNIT (LENGTH_MEASURE( 1.000000000000000082E-05 ), #4533, 'distance_accuracy_value', 'NONE');
#9184 = LINE ( 'NONE', #12846, #23327 ) ;
#9185 = AXIS2_PLACEMENT_3D ( 'NONE', #12469, #6743, #1418 ) ;
#9186 = CARTESIAN_POINT ( 'NONE',  ( 35.00000000000000711, 0.000000000000000000, -100.0000000000000000 ) ) ;
#9187 = EDGE_CURVE ( 'NONE', #1352, #7786, #13074, .T. ) ;
#9188 = EDGE_LOOP ( 'NONE', ( #7047, #16267, #8591, #14492 ) ) ;
#9190 = ADVANCED_FACE ( 'NONE', ( #6821 ), #15663, .F. ) ;
#9189 = PLANE ( 'NONE',  #16054 ) ;
#9191 = ORIENTED_EDGE ( 'NONE', *, *, #15560, .T. ) ;
#9192 = DIRECTION ( 'NONE',  ( 1.000000000000000000, 3.469446951953614189E-16, 0.000000000000000000 ) ) ;
#9194 = VECTOR ( 'NONE', #16718, 1000.000000000000114 ) ;
#9193 = CARTESIAN_POINT ( 'NONE',  ( -4.140404888673278272, -2.228338276487456415, -3.686887068327035166 ) ) ;
#9195 = ORIENTED_EDGE ( 'NONE', *, *, #4827, .T. ) ;
#9196 = PLANE ( 'NONE',  #14654 ) ;
#9197 = CARTESIAN_POINT ( 'NONE',  ( -285.2000000000014666, -129.2000000000000455, -146.4928932188134070 ) ) ;
#9198 = AXIS2_PLACEMENT_3D ( 'NONE', #21509, #21988, #3152 ) ;
#9199 = CARTESIAN_POINT ( 'NONE',  ( -24.83884780301425721, -1003.272451888078649, 145.0000119999999981 ) ) ;
#9200 = AXIS2_PLACEMENT_3D ( 'NONE', #1434, #3137, #3242 ) ;
#9201 = FACE_OUTER_BOUND ( 'NONE', #18344, .T. ) ;
#9202 = CARTESIAN_POINT ( 'NONE',  ( -1.211595439868048629, 7.960739084487649109, -0.4504974108211966533 ) ) ;
#9203 = AXIS2_PLACEMENT_3D ( 'NONE', #14227, #8404, #23129 ) ;
#9204 = CARTESIAN_POINT ( 'NONE',  ( -112.7436279071531828, 91.18044947428913360, 90.00000000000000000 ) ) ;
#9205 = ORIENTED_EDGE ( 'NONE', *, *, #6061, .F. ) ;
#9206 = CARTESIAN_POINT ( 'NONE',  ( -100.0000000000000000, 269.9999999999999432, 125.0000000000000284 ) ) ;
#9207 = DIRECTION ( 'NONE',  ( 1.350636282998972974E-14, 0.000000000000000000, -1.000000000000000000 ) ) ;
#9208 = PRESENTATION_STYLE_ASSIGNMENT (( #1697 ) ) ;
#9210 = VERTEX_POINT ( 'NONE', #17569 ) ;
#9209 = EDGE_LOOP ( 'NONE', ( #23694, #15652, #1961, #13588, #16092 ) ) ;
#9211 = DIRECTION ( 'NONE',  ( 0.000000000000000000, 0.000000000000000000, 1.000000000000000000 ) ) ;
#9212 = CARTESIAN_POINT ( 'NONE',  ( -109.8074641843675749, 85.22886158240835641, -90.00000000000000000 ) ) ;
#9213 = CARTESIAN_POINT ( 'NONE',  ( 280.9952621458755857, 268.9079617568159506, -146.9223300543793016 ) ) ;
#9214 = VERTEX_POINT ( 'NONE', #6463 ) ;
#9215 = AXIS2_PLACEMENT_3D ( 'NONE', #14608, #12837, #14735 ) ;
#9216 = DIRECTION ( 'NONE',  ( 1.000000000000000000, 0.000000000000000000, 0.000000000000000000 ) ) ;
#9217 = ADVANCED_FACE ( 'NONE', ( #13994 ), #21319, .F. ) ;
#9218 = VECTOR ( 'NONE', #12568, 1000.000000000000000 ) ;
#9219 = ORIENTED_EDGE ( 'NONE', *, *, #19441, .F. ) ;
#9220 = EDGE_CURVE ( 'NONE', #14046, #3985, #2733, .T. ) ;
#9221 = AXIS2_PLACEMENT_3D ( 'NONE', #20936, #19237, #11801 ) ;
#9222 = AXIS2_PLACEMENT_3D ( 'NONE', #14709, #9383, #7678 ) ;
#9223 = CYLINDRICAL_SURFACE ( 'NONE', #13831, 2.649999999999999467 ) ;
#9224 = AXIS2_PLACEMENT_3D ( 'NONE', #5564, #3976, #2165 ) ;
#9225 = EDGE_LOOP ( 'NONE', ( #23072, #8365, #21045, #5436 ) ) ;
#9226 = CARTESIAN_POINT ( 'NONE',  ( 5.200000000000002842, 0.000000000000000000, 2.500000000000000444 ) ) ;
#9227 = DIRECTION ( 'NONE',  ( 3.736327486719275871E-16, -1.000000000000000000, 3.469446951953614189E-15 ) ) ;
#9228 = CONICAL_SURFACE ( 'NONE', #11973, 2.055000000000001492, 0.7853981633974633780 ) ;
#9229 = ORIENTED_EDGE ( 'NONE', *, *, #22436, .T. ) ;
#9230 = CARTESIAN_POINT ( 'NONE',  ( 125.4586218058189075, -1091.022788359628976, 28.11255663403414928 ) ) ;
#9231 = ORIENTED_EDGE ( 'NONE', *, *, #7363, .T. ) ;
#9232 = CARTESIAN_POINT ( 'NONE',  ( -127.9021285790841205, 87.55595642181886262, 32.50000000000646594 ) ) ;
#9233 = CARTESIAN_POINT ( 'NONE',  ( 134.1261853992450312, 77.68633335585877830, 29.67072815018523713 ) ) ;
#9234 = CARTESIAN_POINT ( 'NONE',  ( 0.000000000000000000, 0.000000000000000000, -9.974600000000000577 ) ) ;
#9235 = PRODUCT_DEFINITION_SHAPE ( 'NONE', 'NONE',  #1042 ) ;
#9236 = PRESENTATION_LAYER_ASSIGNMENT (  '', '', ( #17334 ) ) ;
#9237 = DIRECTION ( 'NONE',  ( 0.000000000000000000, 0.000000000000000000, -1.000000000000000000 ) ) ;
#9238 = CIRCLE ( 'NONE', #17338, 4.171999999999999709 ) ;
#9239 = FACE_OUTER_BOUND ( 'NONE', #19216, .T. ) ;
#9240 = CIRCLE ( 'NONE', #23499, 21.50000000000000000 ) ;
#9241 = TOROIDAL_SURFACE ( 'NONE', #18473, 4.000000000000000000, 0.2500000000000000000 ) ;
#9242 = CIRCLE ( 'NONE', #10034, 145.0000000000000284 ) ;
#9243 = CIRCLE ( 'NONE', #13889, 145.0000000000000284 ) ;
#9244 = ORIENTED_EDGE ( 'NONE', *, *, #22868, .F. ) ;
#9245 = DIRECTION ( 'NONE',  ( 0.000000000000000000, 0.000000000000000000, 1.000000000000000000 ) ) ;
#9246 = CARTESIAN_POINT ( 'NONE',  ( -7.500000000000000000, 3.608439182435158710, -7.298562697733104621 ) ) ;
#9247 = FACE_OUTER_BOUND ( 'NONE', #14196, .T. ) ;
#9248 =( REPRESENTATION_RELATIONSHIP ('NONE','NONE', #10127, #8847 ) REPRESENTATION_RELATIONSHIP_WITH_TRANSFORMATION ( #19283 )SHAPE_REPRESENTATION_RELATIONSHIP( ) );
#9249 = VERTEX_POINT ( 'NONE', #15902 ) ;
#9250 = DIRECTION ( 'NONE',  ( -0.000000000000000000, -0.000000000000000000, 1.000000000000000000 ) ) ;
#9251 = CARTESIAN_POINT ( 'NONE',  ( 146.0000000000002274, -801.0618695410406644, -29.99999999999356604 ) ) ;
#9252 = CARTESIAN_POINT ( 'NONE',  ( 7.500000000000000888, -2.886751345948134873, -7.198902722707428481 ) ) ;
#9254 = CIRCLE ( 'NONE', #394, 2.499999999999998668 ) ;
#9253 = AXIS2_PLACEMENT_3D ( 'NONE', #12408, #16098, #14186 ) ;
#9255 = DIRECTION ( 'NONE',  ( 1.000000000000000000, 0.000000000000000000, 0.000000000000000000 ) ) ;
#9256 = LINE ( 'NONE', #2094, #8479 ) ;
#9257 = VECTOR ( 'NONE', #11202, 1000.000000000000000 ) ;
#9258 = VERTEX_POINT ( 'NONE', #12185 ) ;
#9259 = VECTOR ( 'NONE', #21388, 1000.000000000000000 ) ;
#9260 = AXIS2_PLACEMENT_3D ( 'NONE', #1982, #18628, #14810 ) ;
#9261 = CIRCLE ( 'NONE', #13918, 2.055000000000001492 ) ;
#9262 = CARTESIAN_POINT ( 'NONE',  ( -1.636246173744689836, -974.9999999999997726, 145.0000119999999697 ) ) ;
#9263 = ORIENTED_EDGE ( 'NONE', *, *, #2409, .F. ) ;
#9264 = CARTESIAN_POINT ( 'NONE',  ( 57.99999999999999289, -135.7851947190609678, -3.814213562373143684 ) ) ;
#9265 = CARTESIAN_POINT ( 'NONE',  ( -79.99999999999995737, -62.00000000000004263, 3.000000000000000000 ) ) ;
#9266 = ORIENTED_EDGE ( 'NONE', *, *, #18137, .F. ) ;
#9267 = CARTESIAN_POINT ( 'NONE',  ( 122.9870427404257498, -1094.335589877584880, -30.66034227022087677 ) ) ;
#9268 = CARTESIAN_POINT ( 'NONE',  ( 34.99999999999999289, 2.055000000000000160, 0.000000000000000000 ) ) ;
#9269 = CARTESIAN_POINT ( 'NONE',  ( 4.000000000000000000, 2.309401076758515803, -0.4999999999999995559 ) ) ;
#9270 = CARTESIAN_POINT ( 'NONE',  ( -37.64999999999999147, 90.00000000000001421, 0.000000000000000000 ) ) ;
#9271 = CARTESIAN_POINT ( 'NONE',  ( 4.024499207728657879, 2.323545700935571556, -3.572172305156506411 ) ) ;
#9272 = CARTESIAN_POINT ( 'NONE',  ( 21.69578997558838651, 12.52876685377504096, 145.0000119999999697 ) ) ;
#9273 = EDGE_LOOP ( 'NONE', ( #19309, #21161, #18920, #12618 ) ) ;
#9274 = ORIENTED_EDGE ( 'NONE', *, *, #22005, .F. ) ;
#9275 = PRODUCT_DEFINITION_FORMATION_WITH_SPECIFIED_SOURCE ( 'ANY', '', #20003, .NOT_KNOWN. ) ;
#9276 = DIRECTION ( 'NONE',  ( -1.000000000000000000, 0.000000000000000000, 0.000000000000000000 ) ) ;
#9277 = LINE ( 'NONE', #10877, #4224 ) ;
#9278 =( GEOMETRIC_REPRESENTATION_CONTEXT ( 3 ) GLOBAL_UNCERTAINTY_ASSIGNED_CONTEXT ( ( #11609 ) ) GLOBAL_UNIT_ASSIGNED_CONTEXT ( ( #3875, #18243, #3389 ) ) REPRESENTATION_CONTEXT ( 'NONE', 'WORKASPACE' ) );
#9279 = AXIS2_PLACEMENT_3D ( 'NONE', #23528, #19523, #17969 ) ;
#9280 = ORIENTED_EDGE ( 'NONE', *, *, #1972, .F. ) ;
#9281 = VECTOR ( 'NONE', #19640, 1000.000000000000000 ) ;
#9282 = VECTOR ( 'NONE', #5758, 1000.000000000000000 ) ;
#9283 = CARTESIAN_POINT ( 'NONE',  ( 3.808017302909278978, 9.322003897477310730, 200.0000120000000550 ) ) ;
#9284 = CARTESIAN_POINT ( 'NONE',  ( -117.3074641843675749, 85.22886158240835641, -90.00000000000000000 ) ) ;
#9285 = B_SPLINE_CURVE_WITH_KNOTS ( 'NONE', 3,
 ( #18608, #20300, #9348, #7276, #14787, #7633, #14670, #159, #3414, #5354, #13124, #11183, #5474, #16707, #10828, #12882, #16816, #9464, #11055, #22115, #7403, #9230, #12776, #18375, #275, #16593, #12644, #1608 ),
 .UNSPECIFIED., .F., .F.,
 ( 4, 2, 2, 2, 2, 2, 2, 2, 2, 2, 2, 2, 2, 4 ),
 ( 0.007862850516742021789, 0.008354729399060772249, 0.008846608281379520974, 0.009830366046016477191, 0.01032224492833494489, 0.01081412381065341086, 0.01130600269297188029, 0.01179788157529034626, 0.01278163933992727125, 0.01327351822224584824, 0.01376539710456442522, 0.01425727598688300221, 0.01474915486920157920, 0.01573291263383920502 ),
 .UNSPECIFIED. ) ;
#9286 = DIRECTION ( 'NONE',  ( 0.000000000000000000, -1.177509268541832635E-16, 1.000000000000000000 ) ) ;
#9287 = ADVANCED_FACE ( 'NONE', ( #19489 ), #2942, .T. ) ;
#9288 = ORIENTED_EDGE ( 'NONE', *, *, #15677, .T. ) ;
#9289 = DIRECTION ( 'NONE',  ( 0.6964005597823107463, -0.7176533009294141507, 6.982962677686266711E-15 ) ) ;
#9290 = ADVANCED_FACE ( 'NONE', ( #23237 ), #6708, .F. ) ;
#9291 = PLANE ( 'NONE',  #23605 ) ;
#9292 = ADVANCED_FACE ( 'NONE', ( #1385 ), #9000, .F. ) ;
#9293 = DIRECTION ( 'NONE',  ( -0.000000000000000000, -1.000000000000000000, -0.000000000000000000 ) ) ;
#9294 = VERTEX_POINT ( 'NONE', #20311 ) ;
#9295 = DIRECTION ( 'NONE',  ( 0.000000000000000000, 0.000000000000000000, 1.000000000000000000 ) ) ;
#9296 = B_SPLINE_CURVE_WITH_KNOTS ( 'NONE', 3,
 ( #14790, #16120, #12532, #22118, #1835, #5594, #14337, #19849, #19960, #3642, #18046, #14550, #3297, #11058, #9233, #18165, #3418, #18379, #16599, #20453, #1373, #12783, #8885, #8760, #23468, #56, #16250, #23594, #1612, #20089, #8993, #12885 ),
 .UNSPECIFIED., .F., .F.,
 ( 4, 2, 2, 2, 2, 2, 2, 2, 2, 2, 2, 2, 2, 2, 2, 4 ),
 ( 0.000000000000000000, 0.0004914281572963739766, 0.0009828563145927479532, 0.001474284471889121930, 0.001965712629185495906, 0.002457140786481870100, 0.002948568943778243859, 0.003931425258371016099, 0.004422853415667405905, 0.004914281572963798313, 0.005405709730260188986, 0.005897137887556580527, 0.006388566044852972067, 0.006879994202149363608, 0.007371422359445755149, 0.007862850516742146689 ),
 .UNSPECIFIED. ) ;
#9297 = CARTESIAN_POINT ( 'NONE',  ( -282.2000000000010687, -19.99999999999898392, 105.0000000000000000 ) ) ;
#9298 = VECTOR ( 'NONE', #9522, 1000.000000000000000 ) ;
#9299 = EDGE_CURVE ( 'NONE', #12117, #16906, #5320, .T. ) ;
#9300 = DIRECTION ( 'NONE',  ( 0.000000000000000000, 0.000000000000000000, -1.000000000000000000 ) ) ;
#9301 = ORIENTED_EDGE ( 'NONE', *, *, #23613, .F. ) ;
#9302 = ORIENTED_EDGE ( 'NONE', *, *, #13501, .T. ) ;
#9303 = DIRECTION ( 'NONE',  ( 0.000000000000000000, -3.495664435217746987E-15, 1.000000000000000000 ) ) ;
#9304 = PRODUCT_CONTEXT ( 'NONE', #21391, 'mechanical' ) ;
#9305 = CARTESIAN_POINT ( 'NONE',  ( -127.4422799395774888, 88.22408193900511719, -32.37389708099360064 ) ) ;
#9306 = CARTESIAN_POINT ( 'NONE',  ( -288.2000000000006708, 90.00000000000102318, -32.35000000000004405 ) ) ;
#9307 = CARTESIAN_POINT ( 'NONE',  ( 2.500000000000000000, -2.357898499370432610, 3.252606517456513302E-15 ) ) ;
#9308 = VERTEX_POINT ( 'NONE', #14688 ) ;
#9309 = CARTESIAN_POINT ( 'NONE',  ( -24.83884780301427853, -3.272451888078302229, 145.0000119999999981 ) ) ;
#9310 = PRODUCT_DEFINITION_CONTEXT ( 'detailed design', #8468, 'design' ) ;
#9311 = ORIENTED_EDGE ( 'NONE', *, *, #9852, .F. ) ;
#9312 = DIRECTION ( 'NONE',  ( 0.6964005597823107463, -0.7176533009294141507, 6.982962677686266711E-15 ) ) ;
#9313 = LINE ( 'NONE', #7593, #9539 ) ;
#9314 = ORIENTED_EDGE ( 'NONE', *, *, #12434, .F. ) ;
#9315 = CARTESIAN_POINT ( 'NONE',  ( -79.99999999999995737, -62.00000000000004263, 0.000000000000000000 ) ) ;
#9316 = EDGE_CURVE ( 'NONE', #16388, #2213, #18404, .T. ) ;
#9317 = EDGE_LOOP ( 'NONE', ( #5277, #10044, #6571, #2006 ) ) ;
#9318 = DIRECTION ( 'NONE',  ( 0.000000000000000000, 0.000000000000000000, 1.000000000000000000 ) ) ;
#9319 = EDGE_CURVE ( 'NONE', #19773, #20769, #21784, .T. ) ;
#9320 = CARTESIAN_POINT ( 'NONE',  ( -175.1609685624536326, -1088.719770019218913, 30.00000000000675726 ) ) ;
#9321 = VERTEX_POINT ( 'NONE', #16360 ) ;
#9322 = LINE ( 'NONE', #127, #8102 ) ;
#9323 = EDGE_CURVE ( 'NONE', #12219, #20656, #2981, .T. ) ;
#9324 = DIRECTION ( 'NONE',  ( 0.000000000000000000, -1.000000000000000000, 0.000000000000000000 ) ) ;
#9325 = CARTESIAN_POINT ( 'NONE',  ( 8.055391459054613179, -1023.723152614744777, 145.0000119999999697 ) ) ;
#9326 = CARTESIAN_POINT ( 'NONE',  ( -281.9771650631954572, 268.7755899421579784, -146.0571594757292075 ) ) ;
#9327 = CARTESIAN_POINT ( 'NONE',  ( 125.9265396616750223, -1090.374350352354895, -30.65604281379834717 ) ) ;
#9328 = ADVANCED_FACE ( 'NONE', ( #7297 ), #18387, .F. ) ;
#9329 = EDGE_CURVE ( 'NONE', #6345, #4760, #10845, .T. ) ;
#9330 = FACE_BOUND ( 'NONE', #19081, .T. ) ;
#9331 = ORIENTED_EDGE ( 'NONE', *, *, #13755, .F. ) ;
#9332 = CARTESIAN_POINT ( 'NONE',  ( -1.500000000000000000, 11.99999999999999822, 200.0000000000000000 ) ) ;
#9333 = CARTESIAN_POINT ( 'NONE',  ( 0.000000000000000000, 0.000000000000000000, -9.999999999999998224 ) ) ;
#9334 =( LENGTH_UNIT ( ) NAMED_UNIT ( * ) SI_UNIT ( .MILLI., .METRE. ) );
#9336 = ORIENTED_EDGE ( 'NONE', *, *, #8132, .T. ) ;
#9335 = ORIENTED_EDGE ( 'NONE', *, *, #13755, .T. ) ;
#9337 = CARTESIAN_POINT ( 'NONE',  ( -293.2000000000010118, 89.99999999999970157, 35.00000000000072475 ) ) ;
#9338 = LINE ( 'NONE', #11290, #16 ) ;
#9339 = CARTESIAN_POINT ( 'NONE',  ( 0.000000000000000000, 0.000000000000000000, 150.0000000000000284 ) ) ;
#9340 = ORIENTED_EDGE ( 'NONE', *, *, #20939, .T. ) ;
#9341 = CARTESIAN_POINT ( 'NONE',  ( -134.5892462183198290, -1076.881310361372016, 30.65375098132850340 ) ) ;
#9342 = EDGE_LOOP ( 'NONE', ( #14179, #17360, #12381, #10186, #11137 ) ) ;
#9343 = DIRECTION ( 'NONE',  ( 0.000000000000000000, 0.000000000000000000, 1.000000000000000000 ) ) ;
#9344 = VERTEX_POINT ( 'NONE', #18173 ) ;
#9345 = CARTESIAN_POINT ( 'NONE',  ( -100.0000000000000000, -1400.000000000000000, -125.0000000000001705 ) ) ;
#9346 = DIRECTION ( 'NONE',  ( 0.000000000000000000, 0.000000000000000000, 1.000000000000000000 ) ) ;
#9347 = ORIENTED_EDGE ( 'NONE', *, *, #16107, .T. ) ;
#9348 = CARTESIAN_POINT ( 'NONE',  ( 124.6651547408757210, -1092.106598813447135, 32.48437713430730156 ) ) ;
#9349 = ORIENTED_EDGE ( 'NONE', *, *, #11440, .T. ) ;
#9350 = CARTESIAN_POINT ( 'NONE',  ( -128.3589811823735545, 86.88495287852394711, 32.37380477188061434 ) ) ;
#9351 = CARTESIAN_POINT ( 'NONE',  ( 2.500000000000000000, -2.357898499370431722, 2.818925648462311528E-15 ) ) ;
#9352 = DIRECTION ( 'NONE',  ( -0.000000000000000000, -0.000000000000000000, 1.000000000000000000 ) ) ;
#9353 = CARTESIAN_POINT ( 'NONE',  ( -64.99999999999997158, -52.79999999999974847, 35.00000000000017764 ) ) ;
#9354 = EDGE_CURVE ( 'NONE', #18546, #12980, #20403, .T. ) ;
#9355 = ADVANCED_FACE ( 'NONE', ( #10714 ), #23708, .T. ) ;
#9356 = DIRECTION ( 'NONE',  ( -1.000000000000000000, -0.000000000000000000, -0.000000000000000000 ) ) ;
#9357 = EDGE_CURVE ( 'NONE', #2323, #5659, #19858, .T. ) ;
#9358 = DIRECTION ( 'NONE',  ( 0.000000000000000000, 0.000000000000000000, 1.000000000000000000 ) ) ;
#9359 = EDGE_LOOP ( 'NONE', ( #561, #552, #20094, #7393 ) ) ;
#9360 = DIRECTION ( 'NONE',  ( 1.000000000000000000, 0.000000000000000000, 0.000000000000000000 ) ) ;
#9361 = DIRECTION ( 'NONE',  ( -0.000000000000000000, -0.000000000000000000, 1.000000000000000000 ) ) ;
#9362 = CARTESIAN_POINT ( 'NONE',  ( 34.75000000000005684, 100.0000000000000000, 150.2000000000009550 ) ) ;
#9363 = ORIENTED_EDGE ( 'NONE', *, *, #15942, .T. ) ;
#9364 = CARTESIAN_POINT ( 'NONE',  ( -285.2000000000010687, -19.99999999999898392, 107.6499999999999631 ) ) ;
#9365 = CARTESIAN_POINT ( 'NONE',  ( -280.6847249064867924, 273.0299999999999159, -145.1244295015775094 ) ) ;
#9366 = AXIS2_PLACEMENT_3D ( 'NONE', #15808, #8202, #15575 ) ;
#9367 = FACE_OUTER_BOUND ( 'NONE', #17550, .T. ) ;
#9368 = CARTESIAN_POINT ( 'NONE',  ( 155.0000000000000284, -210.0000000000003411, -29.99999999999350564 ) ) ;
#9369 = CARTESIAN_POINT ( 'NONE',  ( 281.4301685943533471, 268.1431883566702368, -150.1999999999999318 ) ) ;
#9370 = CONTEXT_DEPENDENT_SHAPE_REPRESENTATION ( #5526, #1206 ) ;
#9371 = VERTEX_POINT ( 'NONE', #16258 ) ;
#9372 = CARTESIAN_POINT ( 'NONE',  ( 2.500000000000002220, 1.178949249685212086, -2.042000000000002036 ) ) ;
#9373 = VERTEX_POINT ( 'NONE', #3773 ) ;
#9374 = CARTESIAN_POINT ( 'NONE',  ( 145.9999999999997726, -209.9999999999996874, 32.05500000000641592 ) ) ;
#9375 = CARTESIAN_POINT ( 'NONE',  ( 34.75000000000005684, 100.0000000000000000, 147.2000000000005855 ) ) ;
#9376 = ORIENTED_EDGE ( 'NONE', *, *, #2891, .T. ) ;
#9377 = CARTESIAN_POINT ( 'NONE',  ( -44.99999999999997868, -52.79999999999937188, 192.3500000000001933 ) ) ;
#9378 = DIRECTION ( 'NONE',  ( 0.000000000000000000, -0.000000000000000000, -1.000000000000000000 ) ) ;
#9379 = CARTESIAN_POINT ( 'NONE',  ( 0.000000000000000000, 0.000000000000000000, 6.500000000000000888 ) ) ;
#9380 = DIRECTION ( 'NONE',  ( 0.000000000000000000, -3.469446951953614583E-15, -1.000000000000000000 ) ) ;
#9381 = EDGE_CURVE ( 'NONE', #21582, #6258, #13821, .T. ) ;
#9382 = FACE_BOUND ( 'NONE', #3663, .T. ) ;
#9383 = DIRECTION ( 'NONE',  ( -1.000000000000000000, -2.775557561562891351E-17, 0.000000000000000000 ) ) ;
#9384 = CARTESIAN_POINT ( 'NONE',  ( -7.500000000000000000, -3.882691789160215290, -7.781695678273567118 ) ) ;
#9385 = AXIS2_PLACEMENT_3D ( 'NONE', #2111, #7921, #9503 ) ;
#9386 = EDGE_CURVE ( 'NONE', #15759, #17675, #16509, .T. ) ;
#9387 = ORIENTED_EDGE ( 'NONE', *, *, #23781, .F. ) ;
#9388 = CARTESIAN_POINT ( 'NONE',  ( -288.2000000000010687, -19.99999999999898392, 105.0000000000000000 ) ) ;
#9389 = CARTESIAN_POINT ( 'NONE',  ( -90.00000000000000000, 3.053113317719180486E-13, 129.9038105676659711 ) ) ;
#9390 = ORIENTED_EDGE ( 'NONE', *, *, #13505, .T. ) ;
#9391 = CARTESIAN_POINT ( 'NONE',  ( 9.999999999999998224, 6.123233995736764310E-16, 200.0000060000000133 ) ) ;
#9392 = LINE ( 'NONE', #14482, #21632 ) ;
#9393 = DIRECTION ( 'NONE',  ( 0.000000000000000000, -1.000000000000000000, 0.000000000000000000 ) ) ;
#9394 = AXIS2_PLACEMENT_3D ( 'NONE', #14789, #55, #18610 ) ;
#9395 = EDGE_LOOP ( 'NONE', ( #14433, #20120, #12494, #8750 ) ) ;
#9396 = CARTESIAN_POINT ( 'NONE',  ( 5.000000000000000000, -3.513898075855356407, 2.028750000000003162 ) ) ;
#9397 = DIRECTION ( 'NONE',  ( 0.000000000000000000, -1.000000000000000000, 0.000000000000000000 ) ) ;
#9398 = AXIS2_PLACEMENT_3D ( 'NONE', #21553, #19733, #9207 ) ;
#9399 = CARTESIAN_POINT ( 'NONE',  ( 9.739726766683158843, -2.617478843592797144, 200.0000120000001402 ) ) ;
#9400 = ORIENTED_EDGE ( 'NONE', *, *, #7485, .T. ) ;
#9401 = CARTESIAN_POINT ( 'NONE',  ( 5.000000000000000000, -2.342598717236900718, 4.057500000000001883 ) ) ;
#9402 = CARTESIAN_POINT ( 'NONE',  ( -136.9530201128892486, -1072.586991580761151, 30.65186413114638952 ) ) ;
#9403 = DIRECTION ( 'NONE',  ( 0.000000000000000000, 0.000000000000000000, 1.000000000000000000 ) ) ;
#9404 = ORIENTED_EDGE ( 'NONE', *, *, #23180, .F. ) ;
#9405 = EDGE_CURVE ( 'NONE', #2992, #12275, #18274, .T. ) ;
#9406 = FACE_OUTER_BOUND ( 'NONE', #22866, .T. ) ;
#9407 = PRODUCT_CONTEXT ( 'NONE', #20150, 'mechanical' ) ;
#9408 = DIRECTION ( 'NONE',  ( -1.000000000000000000, -0.000000000000000000, -0.000000000000000000 ) ) ;
#9409 = FACE_OUTER_BOUND ( 'NONE', #8116, .T. ) ;
#9410 = CARTESIAN_POINT ( 'NONE',  ( 4.000000000000000000, -1.560351142792952617, -0.2242961665059816367 ) ) ;
#9411 = B_SPLINE_CURVE_WITH_KNOTS ( 'NONE', 3,
 ( #21459, #17382, #17722, #12213, #19395, #21103 ),
 .UNSPECIFIED., .F., .F.,
 ( 4, 2, 4 ),
 ( 2.475503369438313607E-07, 0.002222330217055647119, 0.004444412883774350592 ),
 .UNSPECIFIED. ) ;
#9412 = AXIS2_PLACEMENT_3D ( 'NONE', #4945, #16302, #5298 ) ;
#9413 = ORIENTED_EDGE ( 'NONE', *, *, #10982, .F. ) ;
#9414 = VECTOR ( 'NONE', #7854, 1000.000000000000000 ) ;
#9415 = ORIENTED_EDGE ( 'NONE', *, *, #23066, .T. ) ;
#9416 = CARTESIAN_POINT ( 'NONE',  ( 80.00000000000000000, -61.99999999999998579, 3.000000000000000000 ) ) ;
#9417 = EDGE_CURVE ( 'NONE', #7634, #15263, #13469, .T. ) ;
#9418 = EDGE_CURVE ( 'NONE', #20414, #17401, #172, .T. ) ;
#9419 = EDGE_LOOP ( 'NONE', ( #606, #8878, #11350, #14778 ) ) ;
#9420 = LINE ( 'NONE', #15112, #9484 ) ;
#9421 = CARTESIAN_POINT ( 'NONE',  ( 281.4928932188133217, -129.2000000000000455, 152.4000000000014268 ) ) ;
#9422 = ORIENTED_EDGE ( 'NONE', *, *, #17644, .T. ) ;
#9423 = CARTESIAN_POINT ( 'NONE',  ( 0.6169862416622686752, 8.783631307150953305, -7.913704048099833521 ) ) ;
#9424 = CIRCLE ( 'NONE', #2854, 7.500000000000003553 ) ;
#9425 = VERTEX_POINT ( 'NONE', #7645 ) ;
#9426 = AXIS2_PLACEMENT_3D ( 'NONE', #7411, #2192, #1967 ) ;
#9427 = CARTESIAN_POINT ( 'NONE',  ( 155.0000000000000284, -500.0000000000000000, -29.99999999999997158 ) ) ;
#9428 = FACE_OUTER_BOUND ( 'NONE', #6405, .T. ) ;
#9429 = ORIENTED_EDGE ( 'NONE', *, *, #20155, .F. ) ;
#9430 = VECTOR ( 'NONE', #6500, 1000.000000000000000 ) ;
#9431 = CARTESIAN_POINT ( 'NONE',  ( -1.306442393143578462, -8.377108146505394259, -7.792327460285862983 ) ) ;
#9432 = PLANE ( 'NONE',  #19270 ) ;
#9433 =( NAMED_UNIT ( * ) SI_UNIT ( $, .STERADIAN. ) SOLID_ANGLE_UNIT ( ) );
#9434 = DIRECTION ( 'NONE',  ( 0.9396926207859143121, 1.150791560227857665E-16, -0.3420201433256525592 ) ) ;
#9435 = CARTESIAN_POINT ( 'NONE',  ( 145.0000000000000568, -1000.000000000000000, 90.00000000000000000 ) ) ;
#9436 = EDGE_CURVE ( 'NONE', #20709, #2178, #13367, .T. ) ;
#9437 = CARTESIAN_POINT ( 'NONE',  ( 3.680118525130245732, -2.494084732383344605, -0.3507732604232533524 ) ) ;
#9438 = EDGE_LOOP ( 'NONE', ( #19154, #4816, #8550, #7382 ) ) ;
#9439 = CIRCLE ( 'NONE', #7491, 2.041999999999999815 ) ;
#9440 = EDGE_CURVE ( 'NONE', #4056, #12980, #7965, .T. ) ;
#9441 = CARTESIAN_POINT ( 'NONE',  ( 2.500000000000002220, 2.357898499370434386, -3.469446951953614189E-15 ) ) ;
#9442 = DIRECTION ( 'NONE',  ( 1.000000000000000000, 0.000000000000000000, 0.000000000000000000 ) ) ;
#9444 = ORIENTED_EDGE ( 'NONE', *, *, #6605, .T. ) ;
#9443 = ORIENTED_EDGE ( 'NONE', *, *, #21594, .F. ) ;
#9445 = VECTOR ( 'NONE', #6090, 1000.000000000000000 ) ;
#9446 = CARTESIAN_POINT ( 'NONE',  ( -293.2000000000010118, -20.00000000000084555, 104.9999999999998295 ) ) ;
#9447 = DIRECTION ( 'NONE',  ( -0.000000000000000000, 0.4999999999999979461, -0.8660254037844397068 ) ) ;
#9448 = CARTESIAN_POINT ( 'NONE',  ( 280.2488155364688396, 272.8646579186753343, -146.3610889986682366 ) ) ;
#9449 = EDGE_CURVE ( 'NONE', #12183, #16906, #289, .T. ) ;
#9450 = AXIS2_PLACEMENT_3D ( 'NONE', #21276, #23311, #17420 ) ;
#9451 = VERTEX_POINT ( 'NONE', #648 ) ;
#9452 = EDGE_CURVE ( 'NONE', #471, #5229, #7896, .T. ) ;
#9453 = AXIS2_PLACEMENT_3D ( 'NONE', #4905, #4543, #9999 ) ;
#9454 = DIRECTION ( 'NONE',  ( 0.000000000000000000, 0.000000000000000000, -1.000000000000000000 ) ) ;
#9455 = ORIENTED_EDGE ( 'NONE', *, *, #17276, .T. ) ;
#9456 = CARTESIAN_POINT ( 'NONE',  ( -146.0000000000005116, -784.4690652294799520, -29.99999999999356604 ) ) ;
#9457 = EDGE_CURVE ( 'NONE', #18956, #11863, #18905, .T. ) ;
#9458 = ORIENTED_EDGE ( 'NONE', *, *, #10655, .F. ) ;
#9459 = DIRECTION ( 'NONE',  ( 1.000000000000000000, -3.495664435217746987E-15, -0.000000000000000000 ) ) ;
#9460 = DIRECTION ( 'NONE',  ( -1.000000000000000000, 0.000000000000000000, 0.000000000000000000 ) ) ;
#9461 = ITEM_DEFINED_TRANSFORMATION ( 'NONE', 'NONE', #16996,  #11210 ) ;
#9462 = ORIENTED_EDGE ( 'NONE', *, *, #2639, .F. ) ;
#9463 = AXIS2_PLACEMENT_3D ( 'NONE', #22173, #20245, #17977 ) ;
#9464 = CARTESIAN_POINT ( 'NONE',  ( 125.8137507114124531, -1090.531233726929486, 28.88700448195640647 ) ) ;
#9465 = ORIENTED_EDGE ( 'NONE', *, *, #17171, .F. ) ;
#9466 = CARTESIAN_POINT ( 'NONE',  ( -280.4975000228327531, 272.3132312761073877, 147.6054396500290977 ) ) ;
#9467 = DIRECTION ( 'NONE',  ( 1.000000000000000000, 3.469446951953617640E-16, 8.673617379884035472E-17 ) ) ;
#9468 = AXIS2_PLACEMENT_3D ( 'NONE', #15230, #22561, #20631 ) ;
#9469 = CARTESIAN_POINT ( 'NONE',  ( 4.204115023516791005, -1.660442669500199919, -3.602151381774560068 ) ) ;
#9470 = PLANE ( 'NONE',  #22904 ) ;
#9471 = ORIENTED_EDGE ( 'NONE', *, *, #20927, .F. ) ;
#9472 = CARTESIAN_POINT ( 'NONE',  ( -280.9952621458755857, 270.4188186979286570, -149.5436892194421432 ) ) ;
#9473 = CARTESIAN_POINT ( 'NONE',  ( 0.000000000000000000, 0.000000000000000000, 0.000000000000000000 ) ) ;
#9474 = ORIENTED_EDGE ( 'NONE', *, *, #18029, .T. ) ;
#9475 = DIRECTION ( 'NONE',  ( 1.000000000000000000, 0.000000000000000000, 0.000000000000000000 ) ) ;
#9476 = EDGE_CURVE ( 'NONE', #20600, #15247, #15837, .T. ) ;
#9477 = DIRECTION ( 'NONE',  ( 0.000000000000000000, -1.000000000000000000, 0.000000000000000000 ) ) ;
#9478 = AXIS2_PLACEMENT_3D ( 'NONE', #13346, #4113, #11524 ) ;
#9479 = CARTESIAN_POINT ( 'NONE',  ( 279.9999999999999432, 269.9999999999999432, -144.9999999999999716 ) ) ;
#9480 = ADVANCED_FACE ( 'NONE', ( #16960 ), #6076, .T. ) ;
#9481 = DIRECTION ( 'NONE',  ( -0.000000000000000000, 0.000000000000000000, -1.000000000000000000 ) ) ;
#9482 = LINE ( 'NONE', #5963, #4486 ) ;
#9483 = ADVANCED_FACE ( 'NONE', ( #15279, #14918, #17196, #8017, #13254 ), #535, .F. ) ;
#9484 = VECTOR ( 'NONE', #18572, 1000.000000000000000 ) ;
#9485 = EDGE_CURVE ( 'NONE', #7876, #17401, #14676, .T. ) ;
#9486 = CARTESIAN_POINT ( 'NONE',  ( -90.00000000000000000, -74.99999999999998579, 3.000000000000000000 ) ) ;
#9487 = EDGE_CURVE ( 'NONE', #9995, #16958, #12401, .T. ) ;
#9488 = CARTESIAN_POINT ( 'NONE',  ( -280.0000000000000568, 272.9999999999999432, -144.9999999999999716 ) ) ;
#9489 = ORIENTED_EDGE ( 'NONE', *, *, #15221, .T. ) ;
#9490 = DIRECTION ( 'NONE',  ( 1.000000000000000000, 0.000000000000000000, 0.000000000000000000 ) ) ;
#9491 = ORIENTED_EDGE ( 'NONE', *, *, #16363, .F. ) ;
#9492 = DIRECTION ( 'NONE',  ( 1.000000000000000000, 0.000000000000000000, 0.000000000000000000 ) ) ;
#9493 = FACE_BOUND ( 'NONE', #13465, .T. ) ;
#9494 = CIRCLE ( 'NONE', #5999, 2.649999999999999467 ) ;
#9495 = CARTESIAN_POINT ( 'NONE',  ( -79.99999999999995737, -62.00000000000001421, 5.199999999999997513 ) ) ;
#9496 = ORIENTED_EDGE ( 'NONE', *, *, #2472, .T. ) ;
#9497 = DIRECTION ( 'NONE',  ( -1.000000000000000000, 0.000000000000000000, -0.000000000000000000 ) ) ;
#9498 = DIRECTION ( 'NONE',  ( 0.000000000000000000, 0.000000000000000000, 1.000000000000000000 ) ) ;
#9499 = CARTESIAN_POINT ( 'NONE',  ( 158.0000000000000284, -500.0000000000000000, 30.00000000000001421 ) ) ;
#9500 = CARTESIAN_POINT ( 'NONE',  ( 80.00000000000000000, -56.79999999999998295, 5.199999999999978861 ) ) ;
#9501 = DIRECTION ( 'NONE',  ( 1.000000000000000000, 0.000000000000000000, 0.000000000000000000 ) ) ;
#9502 = LINE ( 'NONE', #20227, #17322 ) ;
#9503 = DIRECTION ( 'NONE',  ( 0.000000000000000000, -1.224646799147353454E-16, 1.000000000000000000 ) ) ;
#9504 = ORIENTED_EDGE ( 'NONE', *, *, #12038, .T. ) ;
#9505 = EDGE_CURVE ( 'NONE', #10284, #10987, #4628, .T. ) ;
#9506 = CYLINDRICAL_SURFACE ( 'NONE', #19559, 35.00000000000000711 ) ;
#9507 = CARTESIAN_POINT ( 'NONE',  ( 40.00000000000000000, 100.0000000000000000, 150.2000000000009550 ) ) ;
#9508 = VERTEX_POINT ( 'NONE', #22739 ) ;
#9509 = ORIENTED_EDGE ( 'NONE', *, *, #11867, .T. ) ;
#9510 = DIRECTION ( 'NONE',  ( -1.000000000000000000, -0.000000000000000000, -0.000000000000000000 ) ) ;
#9511 = FACE_OUTER_BOUND ( 'NONE', #12245, .T. ) ;
#9512 = PLANE ( 'NONE',  #1720 ) ;
#9513 = VERTEX_POINT ( 'NONE', #18519 ) ;
#9514 = EDGE_CURVE ( 'NONE', #14837, #10284, #16832, .T. ) ;
#9515 = DIRECTION ( 'NONE',  ( 0.000000000000000000, 0.000000000000000000, -1.000000000000000000 ) ) ;
#9516 = EDGE_CURVE ( 'NONE', #3080, #8456, #6939, .T. ) ;
#9517 = CARTESIAN_POINT ( 'NONE',  ( 6.602753909532903087, 5.319290460493537154, -7.792447862505332168 ) ) ;
#9518 = CARTESIAN_POINT ( 'NONE',  ( -79.99999999999995737, -138.0000000000000284, 3.000000000000000000 ) ) ;
#9519 = ORIENTED_EDGE ( 'NONE', *, *, #7652, .F. ) ;
#9520 = ADVANCED_FACE ( 'NONE', ( #2200 ), #15158, .T. ) ;
#9521 = DIRECTION ( 'NONE',  ( 0.000000000000000000, 0.000000000000000000, -1.000000000000000000 ) ) ;
#9522 = DIRECTION ( 'NONE',  ( -0.000000000000000000, -0.000000000000000000, 1.000000000000000000 ) ) ;
#9523 = CARTESIAN_POINT ( 'NONE',  ( -312.2000000000014666, -129.2000000000000455, 146.4928932188134638 ) ) ;
#9524 = VERTEX_POINT ( 'NONE', #3038 ) ;
#9525 = CARTESIAN_POINT ( 'NONE',  ( 280.2880230824752061, 269.9999999999999432, -145.1244266708878001 ) ) ;
#9526 = CARTESIAN_POINT ( 'NONE',  ( 0.000000000000000000, 0.000000000000000000, -100.0000000000000000 ) ) ;
#9527 = CIRCLE ( 'NONE', #2563, 2.649999999999971934 ) ;
#9528 = DIRECTION ( 'NONE',  ( -1.110223024625157172E-14, 0.000000000000000000, -1.000000000000000000 ) ) ;
#9529 = DIRECTION ( 'NONE',  ( -1.000000000000000000, -0.000000000000000000, -0.000000000000000000 ) ) ;
#9530 = ORIENTED_EDGE ( 'NONE', *, *, #5727, .T. ) ;
#9531 = ORIENTED_EDGE ( 'NONE', *, *, #5830, .T. ) ;
#9532 = DIRECTION ( 'NONE',  ( -0.000000000000000000, -0.000000000000000000, 1.000000000000000000 ) ) ;
#9533 = DIRECTION ( 'NONE',  ( -1.000000000000000000, 0.000000000000000000, -0.000000000000000000 ) ) ;
#9534 = PRODUCT_DEFINITION_CONTEXT ( 'detailed design', #20316, 'design' ) ;
#9535 = AXIS2_PLACEMENT_3D ( 'NONE', #17624, #14043, #1438 ) ;
#9536 = CARTESIAN_POINT ( 'NONE',  ( 194.7499999999997158, -209.9999999999996874, 32.50000000000675726 ) ) ;
#9537 = CARTESIAN_POINT ( 'NONE',  ( -117.3074641843675749, 85.22886158240835641, 90.00000000000000000 ) ) ;
#9538 = ORIENTED_EDGE ( 'NONE', *, *, #17240, .T. ) ;
#9539 = VECTOR ( 'NONE', #11371, 1000.000000000000000 ) ;
#9540 = DIRECTION ( 'NONE',  ( 0.000000000000000000, 0.000000000000000000, 1.000000000000000000 ) ) ;
#9541 = ORIENTED_EDGE ( 'NONE', *, *, #14479, .T. ) ;
#9542 = CARTESIAN_POINT ( 'NONE',  ( 21.00000000000000355, 0.000000000000000000, 0.000000000000000000 ) ) ;
#9543 = DIRECTION ( 'NONE',  ( -0.7232617928448825673, 0.6905739489807055653, 6.982962677686266711E-15 ) ) ;
#9544 = ORIENTED_EDGE ( 'NONE', *, *, #14781, .T. ) ;
#9545 = EDGE_LOOP ( 'NONE', ( #21331, #11457, #1203, #21195 ) ) ;
#9546 = CARTESIAN_POINT ( 'NONE',  ( -128.6141261030693670, 86.50721885637456410, -27.81095155082708459 ) ) ;
#9547 = DIRECTION ( 'NONE',  ( -1.000000000000000000, -0.000000000000000000, -0.000000000000000000 ) ) ;
#9548 = DIRECTION ( 'NONE',  ( -1.000000000000000000, -0.000000000000000000, -0.000000000000000000 ) ) ;
#9549 = VECTOR ( 'NONE', #23393, 1000.000000000000000 ) ;
#9550 = CARTESIAN_POINT ( 'NONE',  ( -282.2000000000006708, 90.00000000000100897, 34.99999999999999289 ) ) ;
#9551 = CARTESIAN_POINT ( 'NONE',  ( 24.99999999999997868, -998.3637538262552198, 145.0000119999999697 ) ) ;
#9552 = CARTESIAN_POINT ( 'NONE',  ( -45.00000000000000000, 272.9999999999999432, 5.249999999999973355 ) ) ;
#9553 = CARTESIAN_POINT ( 'NONE',  ( 2.855764796983346177, -2.970025579236428737, -0.09382832055446485575 ) ) ;
#9554 = ORIENTED_EDGE ( 'NONE', *, *, #17713, .T. ) ;
#9555 = DIRECTION ( 'NONE',  ( -1.000000000000000000, 0.000000000000000000, 0.000000000000000000 ) ) ;
#9556 = AXIS2_PLACEMENT_3D ( 'NONE', #12277, #17665, #1126 ) ;
#9557 = CARTESIAN_POINT ( 'NONE',  ( 126.3653543294811499, 77.28387428943223370, 30.00000000000641620 ) ) ;
#9558 = SURFACE_SIDE_STYLE ('',( #9807 ) ) ;
#9559 = VECTOR ( 'NONE', #12678, 1000.000000000000000 ) ;
#9560 = VECTOR ( 'NONE', #21605, 1000.000000000000000 ) ;
#9562 = ORIENTED_EDGE ( 'NONE', *, *, #7960, .F. ) ;
#9561 = VERTEX_POINT ( 'NONE', #12153 ) ;
#9563 = CARTESIAN_POINT ( 'NONE',  ( -135.8696211158501228, -1074.595399753385209, -32.49999999999353406 ) ) ;
#9564 = CARTESIAN_POINT ( 'NONE',  ( 280.4976310729377929, 272.3699028110927998, -147.6339272673397716 ) ) ;
#9565 = ORIENTED_EDGE ( 'NONE', *, *, #585, .T. ) ;
#9566 = CARTESIAN_POINT ( 'NONE',  ( -135.0388036711513564, -1076.089031023632515, 28.00959664470840593 ) ) ;
#9567 = ORIENTED_EDGE ( 'NONE', *, *, #2002, .F. ) ;
#9568 = AXIS2_PLACEMENT_3D ( 'NONE', #18906, #3925, #4043 ) ;
#9569 = DIRECTION ( 'NONE',  ( 0.000000000000000000, 2.618450529776326854E-15, 1.000000000000000000 ) ) ;
#9570 = ORIENTED_EDGE ( 'NONE', *, *, #21408, .T. ) ;
#9571 = EDGE_CURVE ( 'NONE', #1621, #18546, #19500, .T. ) ;
#9572 = CIRCLE ( 'NONE', #6105, 7.500000000000000000 ) ;
#9573 = DIRECTION ( 'NONE',  ( -1.000000000000000000, 3.495664435217746592E-15, -0.000000000000000000 ) ) ;
#9574 = CIRCLE ( 'NONE', #11150, 2.041999999999999815 ) ;
#9575 =( LENGTH_UNIT ( ) NAMED_UNIT ( * ) SI_UNIT ( .MILLI., .METRE. ) );
#9576 = ADVANCED_FACE ( 'NONE', ( #4741 ), #19454, .F. ) ;
#9577 = EDGE_CURVE ( 'NONE', #880, #9666, #10196, .T. ) ;
#9578 = VECTOR ( 'NONE', #13865, 1000.000000000000000 ) ;
#9579 = EDGE_LOOP ( 'NONE', ( #22910, #106, #19169, #15627, #3047 ) ) ;
#9580 = AXIS2_PLACEMENT_3D ( 'NONE', #7931, #19142, #13536 ) ;
#9581 = DIRECTION ( 'NONE',  ( 1.000000000000000000, 0.000000000000000000, -0.000000000000000000 ) ) ;
#9582 = ORIENTED_EDGE ( 'NONE', *, *, #19903, .F. ) ;
#9583 = CARTESIAN_POINT ( 'NONE',  ( -127.9021285790841205, 87.55595642181887683, 27.50000000000646239 ) ) ;
#9584 = EDGE_CURVE ( 'NONE', #18851, #20911, #19106, .T. ) ;
#9585 = DIRECTION ( 'NONE',  ( -0.000000000000000000, -0.000000000000000000, 1.000000000000000000 ) ) ;
#9586 = CYLINDRICAL_SURFACE ( 'NONE', #20359, 155.0000000000000284 ) ;
#9587 = CARTESIAN_POINT ( 'NONE',  ( 70.00000000000000000, -112.6666666666666714, 144.9999999999999716 ) ) ;
#9588 = VERTEX_POINT ( 'NONE', #2567 ) ;
#9589 = CARTESIAN_POINT ( 'NONE',  ( -280.0000000000000000, 270.0000000000000000, -144.9999999999999716 ) ) ;
#9590 = ORIENTED_EDGE ( 'NONE', *, *, #12294, .F. ) ;
#9591 = CIRCLE ( 'NONE', #719, 2.649999999999999467 ) ;
#9592 = DIRECTION ( 'NONE',  ( 0.9289202219288174023, 0.3702799228849934510, 0.000000000000000000 ) ) ;
#9593 = AXIS2_PLACEMENT_3D ( 'NONE', #10083, #1533, #16282 ) ;
#9594 = CARTESIAN_POINT ( 'NONE',  ( 34.75000000000005684, 100.0000000000000000, 150.2000000000009550 ) ) ;
#9595 = LINE ( 'NONE', #13495, #21994 ) ;
#9596 = AXIS2_PLACEMENT_3D ( 'NONE', #23047, #4829, #1076 ) ;
#9597 = AXIS2_PLACEMENT_3D ( 'NONE', #15977, #21752, #23202 ) ;
#9598 = DIRECTION ( 'NONE',  ( -1.000000000000000000, -0.000000000000000000, -0.000000000000000000 ) ) ;
#9599 = FACE_OUTER_BOUND ( 'NONE', #7217, .T. ) ;
#9600 = EDGE_LOOP ( 'NONE', ( #12740, #9531, #1606, #16502 ) ) ;
#9601 = AXIS2_PLACEMENT_3D ( 'NONE', #19151, #15454, #4059 ) ;
#9602 = DIRECTION ( 'NONE',  ( 1.000000000000000000, 0.000000000000000000, 0.000000000000000000 ) ) ;
#9603 = FACE_OUTER_BOUND ( 'NONE', #5783, .T. ) ;
#9604 = CARTESIAN_POINT ( 'NONE',  ( 124.4701338314438317, -1092.369831568442805, 32.50000000000646594 ) ) ;
#9605 = ITEM_DEFINED_TRANSFORMATION ( 'NONE', 'NONE', #643,  #11210 ) ;
#9606 = VERTEX_POINT ( 'NONE', #11794 ) ;
#9607 = DIRECTION ( 'NONE',  ( 1.000000000000000000, 0.000000000000000000, 0.000000000000000000 ) ) ;
#9608 = VERTEX_POINT ( 'NONE', #21047 ) ;
#9610 = CARTESIAN_POINT ( 'NONE',  ( 125.6044290879531644, 79.19280534549544370, -29.99999999999356604 ) ) ;
#9609 = AXIS2_PLACEMENT_3D ( 'NONE', #5124, #21666, #17924 ) ;
#9611 = CARTESIAN_POINT ( 'NONE',  ( -37.30746418436648071, -137.9031948627975908, -90.00000000000000000 ) ) ;
#9612 = VECTOR ( 'NONE', #15869, 1000.000000000000000 ) ;
#9613 = VECTOR ( 'NONE', #14348, 1000.000000000000000 ) ;
#9614 = VECTOR ( 'NONE', #15069, 1000.000000000000000 ) ;
#9615 = CARTESIAN_POINT ( 'NONE',  ( 2.500000000000000000, -2.357898499370431722, 2.818925648462311528E-15 ) ) ;
#9616 = ADVANCED_FACE ( 'NONE', ( #986 ), #23774, .F. ) ;
#9617 = ORIENTED_EDGE ( 'NONE', *, *, #515, .F. ) ;
#9618 = DIRECTION ( 'NONE',  ( 1.000000000000000000, 0.000000000000000000, 0.000000000000000000 ) ) ;
#9619 = CIRCLE ( 'NONE', #3821, 2.700000000000000622 ) ;
#9620 = VECTOR ( 'NONE', #22818, 1000.000000000000000 ) ;
#9621 = DIRECTION ( 'NONE',  ( -0.000000000000000000, -0.000000000000000000, 1.000000000000000000 ) ) ;
#9622 = EDGE_CURVE ( 'NONE', #1592, #21376, #23088, .T. ) ;
#9623 = DIRECTION ( 'NONE',  ( -1.000000000000000000, 0.000000000000000000, 0.000000000000000000 ) ) ;
#9624 = CARTESIAN_POINT ( 'NONE',  ( 0.000000000000000000, 0.000000000000000000, -9.999999999999998224 ) ) ;
#9625 = CARTESIAN_POINT ( 'NONE',  ( -146.4450000000000784, -784.4690652294805204, 30.00000000000641975 ) ) ;
#9626 = CARTESIAN_POINT ( 'NONE',  ( 0.000000000000000000, 0.000000000000000000, -90.00000000000000000 ) ) ;
#9627 = CYLINDRICAL_SURFACE ( 'NONE', #19780, 23.50000000000000000 ) ;
#9628 = ADVANCED_FACE ( 'NONE', ( #2911 ), #8106, .F. ) ;
#9629 = ORIENTED_EDGE ( 'NONE', *, *, #107, .T. ) ;
#9630 = PRODUCT_DEFINITION ( 'UNKNOWN', '', #1160, #12956 ) ;
#9631 = VECTOR ( 'NONE', #20791, 1000.000000000000000 ) ;
#9632 = FILL_AREA_STYLE_COLOUR ( '', #20393 ) ;
#9633 = DIRECTION ( 'NONE',  ( 0.000000000000000000, -9.256405414277014607E-16, -1.000000000000000000 ) ) ;
#9634 = CARTESIAN_POINT ( 'NONE',  ( 10.00000000000000000, 0.000000000000000000, -50.00000000000000000 ) ) ;
#9635 = ADVANCED_FACE ( 'NONE', ( #8501 ), #15875, .T. ) ;
#9636 = ORIENTED_EDGE ( 'NONE', *, *, #12122, .T. ) ;
#9637 = ORIENTED_EDGE ( 'NONE', *, *, #6978, .T. ) ;
#9638 = CIRCLE ( 'NONE', #5761, 35.00000000000000000 ) ;
#9639 = CARTESIAN_POINT ( 'NONE',  ( 155.0000000000000284, 4.302114220422482383E-15, 0.000000000000000000 ) ) ;
#9640 = DIRECTION ( 'NONE',  ( 0.000000000000000000, 1.000000000000000000, -3.548298019043423769E-15 ) ) ;
#9641 = AXIS2_PLACEMENT_3D ( 'NONE', #3059, #19596, #4520 ) ;
#9642 = VECTOR ( 'NONE', #1228, 1000.000000000000000 ) ;
#9643 = AXIS2_PLACEMENT_3D ( 'NONE', #22772, #8176, #5985 ) ;
#9644 = VECTOR ( 'NONE', #300, 1000.000000000000000 ) ;
#9645 = CARTESIAN_POINT ( 'NONE',  ( 281.6574776399288567, 269.2538215477169956, -145.8086578304521197 ) ) ;
#9646 = AXIS2_PLACEMENT_3D ( 'NONE', #15888, #1364, #6688 ) ;
#9647 = AXIS2_PLACEMENT_3D ( 'NONE', #10513, #6853, #14135 ) ;
#9648 = EDGE_LOOP ( 'NONE', ( #16654, #7255 ) ) ;
#9649 = DIRECTION ( 'NONE',  ( -1.000000000000000000, -0.000000000000000000, -0.000000000000000000 ) ) ;
#9650 = FACE_OUTER_BOUND ( 'NONE', #19725, .T. ) ;
#9651 = CARTESIAN_POINT ( 'NONE',  ( 0.000000000000000000, 0.000000000000000000, -4.000000000000000000 ) ) ;
#9652 = ORIENTED_EDGE ( 'NONE', *, *, #8275, .T. ) ;
#9653 = DIRECTION ( 'NONE',  ( 0.000000000000000000, 0.000000000000000000, 1.000000000000000000 ) ) ;
#9654 = LINE ( 'NONE', #22658, #16921 ) ;
#9655 = UNCERTAINTY_MEASURE_WITH_UNIT (LENGTH_MEASURE( 1.000000000000000082E-05 ), #11540, 'distance_accuracy_value', 'NONE');
#9656 = CARTESIAN_POINT ( 'NONE',  ( -100.0000000000000853, -127.0000000000000568, 150.2000000000014381 ) ) ;
#9657 = ORIENTED_EDGE ( 'NONE', *, *, #23444, .F. ) ;
#9658 = LINE ( 'NONE', #22664, #1094 ) ;
#9659 = FACE_OUTER_BOUND ( 'NONE', #23335, .T. ) ;
#9661 = VECTOR ( 'NONE', #8661, 1000.000000000000000 ) ;
#9660 =( GEOMETRIC_REPRESENTATION_CONTEXT ( 3 ) GLOBAL_UNCERTAINTY_ASSIGNED_CONTEXT ( ( #15109 ) ) GLOBAL_UNIT_ASSIGNED_CONTEXT ( ( #10843, #19735, #7166 ) ) REPRESENTATION_CONTEXT ( 'NONE', 'WORKASPACE' ) );
#9662 = DIRECTION ( 'NONE',  ( 1.000000000000000000, 0.000000000000000000, -0.000000000000000000 ) ) ;
#9663 = AXIS2_PLACEMENT_3D ( 'NONE', #14532, #19827, #21868 ) ;
#9664 = CIRCLE ( 'NONE', #398, 2.649999999999999467 ) ;
#9665 = AXIS2_PLACEMENT_3D ( 'NONE', #18055, #12896, #1503 ) ;
#9666 = VERTEX_POINT ( 'NONE', #12631 ) ;
#9668 = ORIENTED_EDGE ( 'NONE', *, *, #9584, .F. ) ;
#9667 = EDGE_CURVE ( 'NONE', #17506, #14601, #16577, .T. ) ;
#9669 = EDGE_CURVE ( 'NONE', #644, #18629, #12515, .T. ) ;
#9670 = PLANE ( 'NONE',  #23419 ) ;
#9671 = DIRECTION ( 'NONE',  ( -1.000000000000000000, 0.000000000000000000, 0.000000000000000000 ) ) ;
#9672 = ADVANCED_FACE ( 'NONE', ( #4987 ), #16232, .F. ) ;
#9673 = AXIS2_PLACEMENT_3D ( 'NONE', #8781, #18068, #7073 ) ;
#9674 = PLANE ( 'NONE',  #23345 ) ;
#9675 = DIRECTION ( 'NONE',  ( -0.000000000000000000, -1.000000000000000000, 6.123233995736766036E-17 ) ) ;
#9676 = PRODUCT_DEFINITION_FORMATION_WITH_SPECIFIED_SOURCE ( 'ANY', '', #4766, .NOT_KNOWN. ) ;
#9677 = ORIENTED_EDGE ( 'NONE', *, *, #17560, .T. ) ;
#9678 = DIRECTION ( 'NONE',  ( 0.000000000000000000, 0.000000000000000000, 1.000000000000000000 ) ) ;
#9679 = AXIS2_PLACEMENT_3D ( 'NONE', #5432, #10766, #12840 ) ;
#9680 = AXIS2_PLACEMENT_3D ( 'NONE', #15281, #22613, #13369 ) ;
#9681 = VERTEX_POINT ( 'NONE', #14319 ) ;
#9682 = LINE ( 'NONE', #2525, #21010 ) ;
#9683 = DIRECTION ( 'NONE',  ( -1.000000000000000000, 0.000000000000000000, 0.000000000000000000 ) ) ;
#9684 = EDGE_LOOP ( 'NONE', ( #206, #8241 ) ) ;
#9685 = EDGE_LOOP ( 'NONE', ( #21298, #18941, #22264, #5896 ) ) ;
#9686 = CARTESIAN_POINT ( 'NONE',  ( 1.983456134378398743E-14, -52.79999999999986215, 1.831306136874101694E-13 ) ) ;
#9687 = CYLINDRICAL_SURFACE ( 'NONE', #13153, 25.00000000000000000 ) ;
#9688 = DIRECTION ( 'NONE',  ( -0.000000000000000000, 6.982962677686266711E-15, -1.000000000000000000 ) ) ;
#9689 = CARTESIAN_POINT ( 'NONE',  ( -281.9094021484634709, 268.9021437883071712, -145.9954397628183926 ) ) ;
#9690 = DIRECTION ( 'NONE',  ( 3.469446951953614682E-16, -1.000000000000000000, 3.483493295888648978E-15 ) ) ;
#9691 = DIRECTION ( 'NONE',  ( 0.000000000000000000, 0.000000000000000000, -1.000000000000000000 ) ) ;
#9692 = DIRECTION ( 'NONE',  ( 1.000000000000000000, -0.000000000000000000, 0.000000000000000000 ) ) ;
#9693 = ORIENTED_EDGE ( 'NONE', *, *, #11074, .T. ) ;
#9694 = DIRECTION ( 'NONE',  ( -1.000000000000000000, 0.000000000000000000, 0.000000000000000000 ) ) ;
#9695 = DIRECTION ( 'NONE',  ( 0.000000000000000000, 1.224646799147353207E-16, 1.000000000000000000 ) ) ;
#9696 =( NAMED_UNIT ( * ) SI_UNIT ( $, .STERADIAN. ) SOLID_ANGLE_UNIT ( ) );
#9697 = ORIENTED_EDGE ( 'NONE', *, *, #14215, .F. ) ;
#9698 = CARTESIAN_POINT ( 'NONE',  ( -136.8330323738933316, -1072.812977866783285, -28.74099766568594205 ) ) ;
#9699 = CARTESIAN_POINT ( 'NONE',  ( 280.2488155364688396, 269.9427398886703600, -145.5758453455903805 ) ) ;
#9700 = ORIENTED_EDGE ( 'NONE', *, *, #5230, .T. ) ;
#9701 = CARTESIAN_POINT ( 'NONE',  ( 21.68333333333334423, -89.99999999999998579, 3.000000000000001332 ) ) ;
#9702 = ORIENTED_EDGE ( 'NONE', *, *, #17314, .T. ) ;
#9703 = CARTESIAN_POINT ( 'NONE',  ( -85.22886158240879695, 117.3074641843673049, 90.00000000000000000 ) ) ;
#9704 = ORIENTED_EDGE ( 'NONE', *, *, #522, .T. ) ;
#9705 = LINE ( 'NONE', #13350, #3084 ) ;
#9706 = ORIENTED_EDGE ( 'NONE', *, *, #6154, .F. ) ;
#9707 =( REPRESENTATION_RELATIONSHIP ('NONE','NONE', #10127, #18083 ) REPRESENTATION_RELATIONSHIP_WITH_TRANSFORMATION ( #2458 )SHAPE_REPRESENTATION_RELATIONSHIP( ) );
#9708 = DIRECTION ( 'NONE',  ( 0.000000000000000000, 2.618450529776326854E-15, 1.000000000000000000 ) ) ;
#9709 = ORIENTED_EDGE ( 'NONE', *, *, #23209, .T. ) ;
#9710 = DIRECTION ( 'NONE',  ( -3.495664435217746987E-15, 1.000000000000000000, 0.000000000000000000 ) ) ;
#9711 = DIRECTION ( 'NONE',  ( 1.000000000000000000, 0.000000000000000000, 0.000000000000000000 ) ) ;
#9712 = EDGE_CURVE ( 'NONE', #2027, #12103, #21651, .T. ) ;
#9713 = CARTESIAN_POINT ( 'NONE',  ( -56.99999999999995737, -130.5567675943147208, 0.000000000000000000 ) ) ;
#9714 = CARTESIAN_POINT ( 'NONE',  ( 119.9257125005557043, -1087.686723660050802, -29.99999999999356248 ) ) ;
#9715 = ORIENTED_EDGE ( 'NONE', *, *, #3852, .F. ) ;
#9716 = CARTESIAN_POINT ( 'NONE',  ( -281.7484459290826635, 269.1429506979391704, 145.8703180930665440 ) ) ;
#9718 = ORIENTED_EDGE ( 'NONE', *, *, #13348, .F. ) ;
#9717 = ORIENTED_EDGE ( 'NONE', *, *, #4594, .F. ) ;
#9719 = EDGE_CURVE ( 'NONE', #52, #17333, #20071, .T. ) ;
#9720 = DIRECTION ( 'NONE',  ( 0.9423651898111408132, 0.3345860861306287348, -6.982962677686266711E-15 ) ) ;
#9721 = CARTESIAN_POINT ( 'NONE',  ( -105.0000000000000142, 30.00000000000001421, 3.000000000000001332 ) ) ;
#9722 = DIRECTION ( 'NONE',  ( 1.000000000000000000, 0.000000000000000000, 0.000000000000000000 ) ) ;
#9723 = EDGE_CURVE ( 'NONE', #4961, #12056, #5107, .T. ) ;
#9724 = CARTESIAN_POINT ( 'NONE',  ( 281.3520027839447835, 269.5592670532759030, 145.6220388411722695 ) ) ;
#9725 = CARTESIAN_POINT ( 'NONE',  ( -280.0000000000000568, 269.9999999999999432, 145.0000000000000284 ) ) ;
#9726 = VERTEX_POINT ( 'NONE', #10925 ) ;
#9727 = ADVANCED_FACE ( 'NONE', ( #7143 ), #5460, .F. ) ;
#9728 = LINE ( 'NONE', #11683, #16476 ) ;
#9729 = DIRECTION ( 'NONE',  ( 0.000000000000000000, 0.000000000000000000, -1.000000000000000000 ) ) ;
#9730 = CARTESIAN_POINT ( 'NONE',  ( 123.2631315123082345, -1093.974511992576709, 31.53022738271477721 ) ) ;
#9731 = CONTEXT_DEPENDENT_SHAPE_REPRESENTATION ( #20794, #6203 ) ;
#9732 = ORIENTED_EDGE ( 'NONE', *, *, #12259, .F. ) ;
#9733 = CARTESIAN_POINT ( 'NONE',  ( 2.500000000000000000, 2.357898499370433054, -1.951563910473907981E-15 ) ) ;
#9734 = ORIENTED_EDGE ( 'NONE', *, *, #1336, .T. ) ;
#9735 = DIRECTION ( 'NONE',  ( 0.000000000000000000, 0.000000000000000000, 1.000000000000000000 ) ) ;
#9736 = DIRECTION ( 'NONE',  ( 0.000000000000000000, 0.000000000000000000, 1.000000000000000000 ) ) ;
#9737 = ORIENTED_EDGE ( 'NONE', *, *, #11263, .T. ) ;
#9738 = CARTESIAN_POINT ( 'NONE',  ( -288.2000000000010687, -19.99999999999898392, 105.0000000000000000 ) ) ;
#9739 = VERTEX_POINT ( 'NONE', #23448 ) ;
#9740 = CARTESIAN_POINT ( 'NONE',  ( 34.99999999999999289, 90.00000000000000000, 3.000000000000000000 ) ) ;
#9741 = DIRECTION ( 'NONE',  ( -2.238759164535664589E-46, -3.469446951953614189E-15, -1.000000000000000000 ) ) ;
#9742 = DIRECTION ( 'NONE',  ( 0.000000000000000000, 0.000000000000000000, -1.000000000000000000 ) ) ;
#9743 = CARTESIAN_POINT ( 'NONE',  ( 40.00000000000000000, 100.0000000000000000, -125.0000000000000000 ) ) ;
#9744 = CARTESIAN_POINT ( 'NONE',  ( 119.6158142514527327, -1087.367367941136308, 30.00000000000641620 ) ) ;
#9745 = LINE ( 'NONE', #19257, #6147 ) ;
#9746 = CARTESIAN_POINT ( 'NONE',  ( -20.63749999999999929, 2.449293598294705724E-15, 19.99999999999999289 ) ) ;
#9747 = ORIENTED_EDGE ( 'NONE', *, *, #901, .T. ) ;
#9748 = EDGE_CURVE ( 'NONE', #18892, #14056, #17756, .T. ) ;
#9749 = DIRECTION ( 'NONE',  ( 1.000000000000000000, 0.000000000000000000, 0.000000000000000000 ) ) ;
#9750 = DIRECTION ( 'NONE',  ( 0.000000000000000000, 0.000000000000000000, 1.000000000000000000 ) ) ;
#9751 = ORIENTED_EDGE ( 'NONE', *, *, #999, .T. ) ;
#9752 = AXIS2_PLACEMENT_3D ( 'NONE', #9802, #4230, #9691 ) ;
#9753 = ORIENTED_EDGE ( 'NONE', *, *, #20698, .F. ) ;
#9754 = DIRECTION ( 'NONE',  ( 0.000000000000000000, -0.5000000000000011102, -0.8660254037844379305 ) ) ;
#9755 = CARTESIAN_POINT ( 'NONE',  ( 2.500000000000000000, 1.178949249685217415, 2.041999999999998483 ) ) ;
#9756 = ADVANCED_FACE ( 'NONE', ( #18151 ), #18363, .F. ) ;
#9757 = DIRECTION ( 'NONE',  ( 0.000000000000000000, -0.5000000000000011102, -0.8660254037844379305 ) ) ;
#9758 = EDGE_CURVE ( 'NONE', #8622, #9561, #16974, .T. ) ;
#9759 = ORIENTED_EDGE ( 'NONE', *, *, #9852, .T. ) ;
#9760 = CARTESIAN_POINT ( 'NONE',  ( 124.4701338314438317, -1092.369831568442805, 32.50000000000646594 ) ) ;
#9761 = DIRECTION ( 'NONE',  ( 0.000000000000000000, 0.000000000000000000, -1.000000000000000000 ) ) ;
#9762 = EDGE_CURVE ( 'NONE', #7620, #3485, #762, .T. ) ;
#9763 = LINE ( 'NONE', #19147, #21172 ) ;
#9764 = EDGE_LOOP ( 'NONE', ( #18006, #8001, #14614 ) ) ;
#9765 = CARTESIAN_POINT ( 'NONE',  ( 279.9999999999999432, 267.7999999999999545, 146.4928932188134922 ) ) ;
#9766 = DIRECTION ( 'NONE',  ( 0.000000000000000000, 0.000000000000000000, 1.000000000000000000 ) ) ;
#9767 = ADVANCED_FACE ( 'NONE', ( #14655 ), #19709, .F. ) ;
#9768 = DIRECTION ( 'NONE',  ( -1.000000000000000000, -0.000000000000000000, -0.000000000000000000 ) ) ;
#9769 = EDGE_LOOP ( 'NONE', ( #8942, #21106, #12127, #1952, #22281, #17918 ) ) ;
#9770 = DIRECTION ( 'NONE',  ( -1.000000000000000000, 0.000000000000000000, -0.000000000000000000 ) ) ;
#9771 = SHAPE_REPRESENTATION ( 'head cover', ( #11210 ), #1924 ) ;
#9772 = AXIS2_PLACEMENT_3D ( 'NONE', #23262, #1290, #1181 ) ;
#9773 = CARTESIAN_POINT ( 'NONE',  ( 17.00000000000000000, 0.000000000000000000, 0.000000000000000000 ) ) ;
#9774 = DIRECTION ( 'NONE',  ( -0.7071067811865320296, 9.875400524328840493E-15, 0.7071067811865631159 ) ) ;
#9775 = LINE ( 'NONE', #6013, #1646 ) ;
#9776 = ORIENTED_EDGE ( 'NONE', *, *, #8245, .F. ) ;
#9777 = EDGE_LOOP ( 'NONE', ( #16817, #10659, #14772, #13700 ) ) ;
#9778 = CARTESIAN_POINT ( 'NONE',  ( 7.497491405671719455, 144.8060344827586334, -90.00000000000000000 ) ) ;
#9779 = CARTESIAN_POINT ( 'NONE',  ( 121.5574576620405480, -79.04925354955113903, 90.00000000000000000 ) ) ;
#9780 = AXIS2_PLACEMENT_3D ( 'NONE', #1226, #6901, #14304 ) ;
#9781 = EDGE_CURVE ( 'NONE', #14870, #6737, #1703, .T. ) ;
#9782 = ORIENTED_EDGE ( 'NONE', *, *, #22707, .T. ) ;
#9783 = DIRECTION ( 'NONE',  ( 0.000000000000000000, -1.110223024625156540E-16, 1.000000000000000000 ) ) ;
#9784 = CARTESIAN_POINT ( 'NONE',  ( 2.500000000000000000, -2.357898499370431722, 2.818925648462311528E-15 ) ) ;
#9785 = VERTEX_POINT ( 'NONE', #21760 ) ;
#9786 = EDGE_CURVE ( 'NONE', #13791, #10471, #1162, .T. ) ;
#9787 = DIRECTION ( 'NONE',  ( -0.000000000000000000, -0.000000000000000000, 1.000000000000000000 ) ) ;
#9788 = ORIENTED_EDGE ( 'NONE', *, *, #1652, .T. ) ;
#9789 = EDGE_CURVE ( 'NONE', #16847, #19722, #5223, .T. ) ;
#9790 = DIRECTION ( 'NONE',  ( -1.000000000000000000, -0.000000000000000000, -0.000000000000000000 ) ) ;
#9791 = EDGE_CURVE ( 'NONE', #2320, #20139, #8735, .T. ) ;
#9792 = CARTESIAN_POINT ( 'NONE',  ( 70.00000000000000000, -87.33333333333332860, 145.0000000000000000 ) ) ;
#9793 = ORIENTED_EDGE ( 'NONE', *, *, #14358, .F. ) ;
#9794 = VERTEX_POINT ( 'NONE', #43 ) ;
#9795 = CARTESIAN_POINT ( 'NONE',  ( 4.203833317240879275, 1.627343821129582979, -3.597273115243889929 ) ) ;
#9796 = VECTOR ( 'NONE', #18693, 1000.000000000000000 ) ;
#9797 = DIRECTION ( 'NONE',  ( 0.000000000000000000, 0.000000000000000000, -1.000000000000000000 ) ) ;
#9798 = CIRCLE ( 'NONE', #10967, 5.249999999999973355 ) ;
#9799 = CARTESIAN_POINT ( 'NONE',  ( -11.08413645907697820, -1022.468658677994995, -145.0000000000001137 ) ) ;
#9800 = CARTESIAN_POINT ( 'NONE',  ( 283.7968359015656006, 271.3570580646228336, 145.7774350431395760 ) ) ;
#9801 = LINE ( 'NONE', #3973, #20399 ) ;
#9802 = CARTESIAN_POINT ( 'NONE',  ( 2.700000000000001066, 0.000000000000000000, 0.000000000000000000 ) ) ;
#9803 = CARTESIAN_POINT ( 'NONE',  ( -312.2000000000014666, -132.2000000000000455, 146.4928932188134638 ) ) ;
#9804 = ORIENTED_EDGE ( 'NONE', *, *, #9891, .F. ) ;
#9805 = PLANE ( 'NONE',  #23795 ) ;
#9806 = CARTESIAN_POINT ( 'NONE',  ( 0.3483149870578491347, -8.861353789385031376, -7.493854785173814648 ) ) ;
#9807 = SURFACE_STYLE_FILL_AREA ( #7862 ) ;
#9808 = ORIENTED_EDGE ( 'NONE', *, *, #3009, .F. ) ;
#9809 = DIRECTION ( 'NONE',  ( 0.000000000000000000, 1.000000000000000000, -1.224646799147353207E-16 ) ) ;
#9810 = CARTESIAN_POINT ( 'NONE',  ( -7.497491405671719455, -144.8060344827586334, -90.00000000000000000 ) ) ;
#9811 = VERTEX_POINT ( 'NONE', #7388 ) ;
#9812 = VECTOR ( 'NONE', #14362, 999.9999999999998863 ) ;
#9813 = EDGE_CURVE ( 'NONE', #6807, #21004, #21215, .T. ) ;
#9814 = CARTESIAN_POINT ( 'NONE',  ( -134.8087563975452667, -1076.495802945234345, 31.53271418707683793 ) ) ;
#9815 = AXIS2_PLACEMENT_3D ( 'NONE', #23514, #14369, #1748 ) ;
#9816 = EDGE_LOOP ( 'NONE', ( #18568, #16887, #17535, #2816 ) ) ;
#9817 = CARTESIAN_POINT ( 'NONE',  ( 7.500000000000000888, 3.639598441879751345, -0.7155132341745285007 ) ) ;
#9818 = DIRECTION ( 'NONE',  ( 1.000000000000000000, 0.000000000000000000, 0.000000000000000000 ) ) ;
#9819 = ORIENTED_EDGE ( 'NONE', *, *, #14261, .F. ) ;
#9820 = EDGE_CURVE ( 'NONE', #12981, #21305, #258, .T. ) ;
#9821 = CARTESIAN_POINT ( 'NONE',  ( 3.000000000000002665, 0.000000000000000000, 0.000000000000000000 ) ) ;
#9822 =( NAMED_UNIT ( * ) SI_UNIT ( $, .STERADIAN. ) SOLID_ANGLE_UNIT ( ) );
#9823 = CONTEXT_DEPENDENT_SHAPE_REPRESENTATION ( #22666, #19498 ) ;
#9824 = VERTEX_POINT ( 'NONE', #22465 ) ;
#9825 = EDGE_CURVE ( 'NONE', #22918, #12463, #4104, .T. ) ;
#9826 = DIRECTION ( 'NONE',  ( -1.000000000000000000, 0.000000000000000000, 0.000000000000000000 ) ) ;
#9827 = ORIENTED_EDGE ( 'NONE', *, *, #490, .F. ) ;
#9828 = DIRECTION ( 'NONE',  ( 0.000000000000000000, 1.000000000000000000, -4.183096374613631247E-18 ) ) ;
#9829 = CARTESIAN_POINT ( 'NONE',  ( 0.6250000000000013323, 8.299410119600871383, -7.298562697733108173 ) ) ;
#9830 = LINE ( 'NONE', #2998, #8824 ) ;
#9831 = CIRCLE ( 'NONE', #5568, 0.2000000000000000944 ) ;
#9832 = AXIS2_PLACEMENT_3D ( 'NONE', #17220, #2590, #13641 ) ;
#9833 = DIRECTION ( 'NONE',  ( 0.000000000000000000, 0.000000000000000000, 1.000000000000000000 ) ) ;
#9834 = EDGE_LOOP ( 'NONE', ( #17408, #9229, #10762, #4414 ) ) ;
#9835 = CARTESIAN_POINT ( 'NONE',  ( -280.1244294735509470, 273.0000000000000000, -145.6807971656549796 ) ) ;
#9837 = EDGE_LOOP ( 'NONE', ( #6096, #23109, #12406, #6205 ) ) ;
#9836 = ORIENTED_EDGE ( 'NONE', *, *, #3694, .T. ) ;
#9838 = VECTOR ( 'NONE', #4780, 1000.000000000000000 ) ;
#9839 = CARTESIAN_POINT ( 'NONE',  ( -163.0000000000005400, -784.4690652294797246, -29.99999999999344880 ) ) ;
#9840 = CARTESIAN_POINT ( 'NONE',  ( 0.000000000000000000, 0.000000000000000000, -90.00000000000000000 ) ) ;
#9841 = CARTESIAN_POINT ( 'NONE',  ( 131.7935180829131809, 81.58110848117762259, -28.46728581292316917 ) ) ;
#9842 = CARTESIAN_POINT ( 'NONE',  ( 285.2299999999999045, 267.7999999999999545, 146.4928932188134922 ) ) ;
#9843 = DIRECTION ( 'NONE',  ( 2.220299922379603824E-16, 1.000000000000000000, 0.000000000000000000 ) ) ;
#9844 = ORIENTED_EDGE ( 'NONE', *, *, #18044, .T. ) ;
#9845 = APPLICATION_CONTEXT ( 'automotive_design' ) ;
#9846 = DIRECTION ( 'NONE',  ( -0.000000000000000000, -0.000000000000000000, 1.000000000000000000 ) ) ;
#9847 = AXIS2_PLACEMENT_3D ( 'NONE', #12937, #1890, #12829 ) ;
#9848 = CARTESIAN_POINT ( 'NONE',  ( 287.4000000000013415, -127.0000000000000568, -146.4928932188134070 ) ) ;
#9849 = CARTESIAN_POINT ( 'NONE',  ( 124.3711180590063634, -1092.503257236081254, 27.50000000000645528 ) ) ;
#9850 = ITEM_DEFINED_TRANSFORMATION ( 'NONE', 'NONE', #393,  #11210 ) ;
#9851 = ORIENTED_EDGE ( 'NONE', *, *, #23412, .T. ) ;
#9852 = EDGE_CURVE ( 'NONE', #18604, #20252, #15009, .T. ) ;
#9853 = CARTESIAN_POINT ( 'NONE',  ( -281.4928932188135491, -132.2000000000000455, 152.4000000000014268 ) ) ;
#9854 = ORIENTED_EDGE ( 'NONE', *, *, #4146, .T. ) ;
#9855 = VECTOR ( 'NONE', #5440, 1000.000000000000000 ) ;
#9856 = DIRECTION ( 'NONE',  ( 3.495664435217746592E-15, 1.000000000000000000, 7.709882115452476934E-17 ) ) ;
#9857 = DIRECTION ( 'NONE',  ( 1.000000000000000000, 0.000000000000000000, 0.000000000000000000 ) ) ;
#9858 = VERTEX_POINT ( 'NONE', #395 ) ;
#9859 = CARTESIAN_POINT ( 'NONE',  ( 19.87444003266270087, 15.25452100728112015, -145.0000000000000000 ) ) ;
#9860 = ORIENTED_EDGE ( 'NONE', *, *, #10950, .F. ) ;
#9861 = CARTESIAN_POINT ( 'NONE',  ( 0.000000000000000000, 0.000000000000000000, -177.2000000000013529 ) ) ;
#9862 = CARTESIAN_POINT ( 'NONE',  ( 34.99999999999999289, 90.00000000000000000, 3.000000000000001332 ) ) ;
#9863 = CARTESIAN_POINT ( 'NONE',  ( 119.6158142514527185, -1087.367367941136308, 32.05500000000641592 ) ) ;
#9864 = PLANE ( 'NONE',  #9832 ) ;
#9865 = CARTESIAN_POINT ( 'NONE',  ( -282.2000000000011255, -29.99999999999898037, -102.3500000000000227 ) ) ;
#9866 = AXIS2_PLACEMENT_3D ( 'NONE', #7725, #6018, #17259 ) ;
#9867 = DIRECTION ( 'NONE',  ( -0.000000000000000000, -0.000000000000000000, 1.000000000000000000 ) ) ;
#9868 = CARTESIAN_POINT ( 'NONE',  ( -7.500000000000000000, 1.644753667986373458, -7.029983668655349405 ) ) ;
#9869 = VERTEX_POINT ( 'NONE', #18833 ) ;
#9870 = FACE_BOUND ( 'NONE', #1578, .T. ) ;
#9871 = DIRECTION ( 'NONE',  ( -1.000000000000000000, 3.051161311199799893E-31, 8.144298233840332611E-17 ) ) ;
#9872 = VERTEX_POINT ( 'NONE', #20289 ) ;
#9873 = ORIENTED_EDGE ( 'NONE', *, *, #11595, .T. ) ;
#9874 = AXIS2_PLACEMENT_3D ( 'NONE', #23029, #1302, #8442 ) ;
#9875 = FACE_OUTER_BOUND ( 'NONE', #7819, .T. ) ;
#9876 = CARTESIAN_POINT ( 'NONE',  ( -288.2000000000008981, 30.00000000000101963, -107.6499999999999773 ) ) ;
#9878 = CARTESIAN_POINT ( 'NONE',  ( 80.00000000000000000, -62.00000000000001421, 5.199999999999997513 ) ) ;
#9877 = PRODUCT_DEFINITION_SHAPE ( 'NONE', 'NONE',  #23865 ) ;
#9879 = EDGE_LOOP ( 'NONE', ( #9917, #4180, #7013, #6931 ) ) ;
#9880 = VECTOR ( 'NONE', #15295, 1000.000000000000000 ) ;
#9881 = CARTESIAN_POINT ( 'NONE',  ( -3.679171394226034675, -2.494631558665844739, -0.3503314178412558211 ) ) ;
#9882 = FACE_OUTER_BOUND ( 'NONE', #9925, .T. ) ;
#9883 = EDGE_CURVE ( 'NONE', #4175, #16275, #22220, .T. ) ;
#9884 = DIRECTION ( 'NONE',  ( 0.000000000000000000, 0.000000000000000000, 1.000000000000000000 ) ) ;
#9885 = VERTEX_POINT ( 'NONE', #2173 ) ;
#9886 = EDGE_CURVE ( 'NONE', #22288, #8566, #3931, .T. ) ;
#9887 = CARTESIAN_POINT ( 'NONE',  ( 280.2489140339769165, 272.8335297745771300, 146.3488036478619563 ) ) ;
#9888 = CIRCLE ( 'NONE', #22191, 0.2500000000000002220 ) ;
#9889 = CARTESIAN_POINT ( 'NONE',  ( 0.000000000000000000, -2.357898499370430834, 3.469446951953614189E-15 ) ) ;
#9890 = FACE_OUTER_BOUND ( 'NONE', #23544, .T. ) ;
#9891 = EDGE_CURVE ( 'NONE', #22443, #3284, #9338, .T. ) ;
#9892 = EDGE_LOOP ( 'NONE', ( #11751, #860 ) ) ;
#9893 = CARTESIAN_POINT ( 'NONE',  ( -42.98333333333330586, -89.99999999999997158, 0.000000000000000000 ) ) ;
#9894 = CIRCLE ( 'NONE', #17962, 5.249999999999991118 ) ;
#9895 = APPLICATION_PROTOCOL_DEFINITION ( 'draft international standard', 'automotive_design', 1998, #8468 ) ;
#9896 = DIRECTION ( 'NONE',  ( -3.495664435217746987E-15, -1.000000000000000000, 0.000000000000000000 ) ) ;
#9897 =( REPRESENTATION_RELATIONSHIP ('NONE','NONE', #10127, #22995 ) REPRESENTATION_RELATIONSHIP_WITH_TRANSFORMATION ( #7766 )SHAPE_REPRESENTATION_RELATIONSHIP( ) );
#9898 = EDGE_CURVE ( 'NONE', #16414, #15690, #16926, .T. ) ;
#9900 = ADVANCED_FACE ( 'NONE', ( #20533 ), #18712, .F. ) ;
#9899 = CARTESIAN_POINT ( 'NONE',  ( 0.000000000000000000, 0.000000000000000000, -150.2000000000008981 ) ) ;
#9901 = DIRECTION ( 'NONE',  ( -0.5000000000000034417, 1.060575238724904696E-16, -0.8660254037844367092 ) ) ;
#9902 = VERTEX_POINT ( 'NONE', #11518 ) ;
#9903 = ORIENTED_EDGE ( 'NONE', *, *, #8579, .F. ) ;
#9904 = DIRECTION ( 'NONE',  ( 1.000000000000000000, 0.000000000000000000, 0.000000000000000000 ) ) ;
#9905 = DIRECTION ( 'NONE',  ( 0.000000000000000000, 0.000000000000000000, -1.000000000000000000 ) ) ;
#9906 = EDGE_CURVE ( 'NONE', #3759, #10418, #8884, .T. ) ;
#9907 = ORIENTED_EDGE ( 'NONE', *, *, #23141, .T. ) ;
#9908 = CARTESIAN_POINT ( 'NONE',  ( 1.500000000000000000, 0.000000000000000000, -50.00000000000000000 ) ) ;
#9909 = CARTESIAN_POINT ( 'NONE',  ( -146.0000000000005684, -206.5240652294800725, -29.99999999999356604 ) ) ;
#9910 = ORIENTED_EDGE ( 'NONE', *, *, #15527, .F. ) ;
#9911 = CARTESIAN_POINT ( 'NONE',  ( 85.22886158240964960, -117.3074641843666370, -90.00000000000000000 ) ) ;
#9912 = ORIENTED_EDGE ( 'NONE', *, *, #6359, .F. ) ;
#9913 = VECTOR ( 'NONE', #263, 1000.000000000000000 ) ;
#9914 = DIRECTION ( 'NONE',  ( 0.000000000000000000, 0.000000000000000000, 1.000000000000000000 ) ) ;
#9915 = FACE_OUTER_BOUND ( 'NONE', #1918, .T. ) ;
#9916 = ORIENTED_EDGE ( 'NONE', *, *, #1150, .T. ) ;
#9917 = ORIENTED_EDGE ( 'NONE', *, *, #17971, .F. ) ;
#9918 = CARTESIAN_POINT ( 'NONE',  ( 4.175002511812151873, 2.208363329454889445, -3.469254087858244073 ) ) ;
#9919 = DIRECTION ( 'NONE',  ( 0.000000000000000000, -1.000000000000000000, 1.287488025362403787E-15 ) ) ;
#9920 = ADVANCED_FACE ( 'NONE', ( #4809 ), #12220, .F. ) ;
#9921 = DIRECTION ( 'NONE',  ( -0.000000000000000000, -0.000000000000000000, 1.000000000000000000 ) ) ;
#9922 = CARTESIAN_POINT ( 'NONE',  ( 2.623433461001182909, -7.604994000793866782, -7.633824513837117465 ) ) ;
#9923 = EDGE_CURVE ( 'NONE', #10380, #21139, #19669, .T. ) ;
#9924 = CARTESIAN_POINT ( 'NONE',  ( 145.9999999999998295, -209.9999999999996874, 27.94500000000641649 ) ) ;
#9925 = EDGE_LOOP ( 'NONE', ( #9570, #23058, #22459, #13401 ) ) ;
#9926 = ADVANCED_FACE ( 'NONE', ( #6855 ), #1417, .T. ) ;
#9927 = CARTESIAN_POINT ( 'NONE',  ( -0.3306966981848578069, -8.469326210127253063, -7.349897473154448413 ) ) ;
#9928 = CIRCLE ( 'NONE', #17610, 2.649999999999985700 ) ;
#9929 = EDGE_CURVE ( 'NONE', #1131, #15709, #6989, .T. ) ;
#9930 = EDGE_LOOP ( 'NONE', ( #13703, #11808, #12810, #22851 ) ) ;
#9931 = ADVANCED_FACE ( 'NONE', ( #14378 ), #8835, .F. ) ;
#9932 = DIRECTION ( 'NONE',  ( 0.000000000000000000, 0.000000000000000000, 1.000000000000000000 ) ) ;
#9933 = AXIS2_PLACEMENT_3D ( 'NONE', #6024, #22441, #16778 ) ;
#9934 = FACE_BOUND ( 'NONE', #9892, .T. ) ;
#9935 = EDGE_CURVE ( 'NONE', #4937, #6640, #12736, .T. ) ;
#9936 = ORIENTED_EDGE ( 'NONE', *, *, #18314, .T. ) ;
#9937 = CARTESIAN_POINT ( 'NONE',  ( 5.200000000000020606, 0.000000000000000000, -6.938893903907228378E-15 ) ) ;
#9938 = ORIENTED_EDGE ( 'NONE', *, *, #19363, .T. ) ;
#9939 = DIRECTION ( 'NONE',  ( 0.000000000000000000, 0.000000000000000000, 1.000000000000000000 ) ) ;
#9940 = DIRECTION ( 'NONE',  ( 1.000000000000000000, 0.000000000000000000, 0.000000000000000000 ) ) ;
#9941 = EDGE_LOOP ( 'NONE', ( #20109, #11079 ) ) ;
#9942 = CARTESIAN_POINT ( 'NONE',  ( -281.4928932188135491, 267.7999999999999545, 150.2299999999999898 ) ) ;
#9943 = CARTESIAN_POINT ( 'NONE',  ( 117.3074641843663386, 85.22886158241004750, -90.00000000000000000 ) ) ;
#9944 = AXIS2_PLACEMENT_3D ( 'NONE', #19294, #16160, #19649 ) ;
#9945 = ORIENTED_EDGE ( 'NONE', *, *, #20772, .F. ) ;
#9946 = UNCERTAINTY_MEASURE_WITH_UNIT (LENGTH_MEASURE( 1.000000000000000082E-05 ), #2539, 'distance_accuracy_value', 'NONE');
#9947 = PLANE ( 'NONE',  #17203 ) ;
#9948 = AXIS2_PLACEMENT_3D ( 'NONE', #3577, #5519, #18425 ) ;
#9949 = CARTESIAN_POINT ( 'NONE',  ( -158.1195828810602109, 116.4077317428687479, -27.49999999999322498 ) ) ;
#9950 = CONICAL_SURFACE ( 'NONE', #18394, 2.500000000000000888, 0.9599310885968785900 ) ;
#9951 = PLANE ( 'NONE',  #23453 ) ;
#9952 = DIRECTION ( 'NONE',  ( 5.551115123125785858E-15, 0.000000000000000000, -1.000000000000000000 ) ) ;
#9953 = VERTEX_POINT ( 'NONE', #8564 ) ;
#9954 = DIRECTION ( 'NONE',  ( 1.000000000000000000, 0.000000000000000000, 0.000000000000000000 ) ) ;
#9955 = SURFACE_STYLE_FILL_AREA ( #22958 ) ;
#9957 = ORIENTED_EDGE ( 'NONE', *, *, #14183, .T. ) ;
#9956 = VERTEX_POINT ( 'NONE', #12580 ) ;
#9958 = DIRECTION ( 'NONE',  ( 0.000000000000000000, 0.000000000000000000, 1.000000000000000000 ) ) ;
#9959 = ADVANCED_FACE ( 'NONE', ( #5063 ), #21604, .F. ) ;
#9960 = DIRECTION ( 'NONE',  ( -1.000000000000000000, 0.000000000000000000, 0.000000000000000000 ) ) ;
#9961 = ADVANCED_FACE ( 'NONE', ( #12468 ), #6178, .F. ) ;
#9962 = CARTESIAN_POINT ( 'NONE',  ( 232.0000000000000568, -557.0000000000000000, 0.000000000000000000 ) ) ;
#9963 = DIRECTION ( 'NONE',  ( 1.000000000000000000, -0.000000000000000000, 6.982962677686266711E-15 ) ) ;
#9964 = CIRCLE ( 'NONE', #6081, 2.200000000000028155 ) ;
#9965 = ORIENTED_EDGE ( 'NONE', *, *, #8485, .T. ) ;
#9966 = AXIS2_PLACEMENT_3D ( 'NONE', #2963, #19639, #8920 ) ;
#9967 = CARTESIAN_POINT ( 'NONE',  ( -69.99999999999997158, -87.33333333333338544, 148.0000000000000000 ) ) ;
#9968 = AXIS2_PLACEMENT_3D ( 'NONE', #7035, #5108, #23684 ) ;
#9969 = B_SPLINE_CURVE_WITH_KNOTS ( 'NONE', 3,
 ( #9107, #16710, #16946, #20088, #7514, #7770, #20189, #7278, #22016, #5476, #12884, #3641, #17424, #6197, #22483, #17184, #11534, #975, #15511, #6065, #13832, #4497, #5946, #22837, #755, #8006, #13355, #15620, #20669, #13482, #864, #21155, #8244, #8354 ),
 .UNSPECIFIED., .F., .F.,
 ( 4, 2, 2, 2, 2, 2, 2, 2, 2, 2, 2, 2, 2, 2, 2, 2, 4 ),
 ( 0.2500000000000000000, 0.2812500000000000000, 0.3125000000000000000, 0.3437500000000000000, 0.3750000000000000000, 0.4062500000000000000, 0.4375000000000000000, 0.4687500000000000000, 0.5000000000000000000, 0.5312500000000000000, 0.5625000000000000000, 0.5937500000000000000, 0.6250000000000000000, 0.6562500000000000000, 0.6875000000000000000, 0.7187500000000000000, 0.7500000000000000000 ),
 .UNSPECIFIED. ) ;
#9970 = PLANE ( 'NONE',  #18450 ) ;
#9971 = CARTESIAN_POINT ( 'NONE',  ( 123.9851406373745704, -1093.019934698474117, 27.62610291900636739 ) ) ;
#9972 = CONTEXT_DEPENDENT_SHAPE_REPRESENTATION ( #11617, #4271 ) ;
#9973 = VERTEX_POINT ( 'NONE', #18091 ) ;
#9974 = LINE ( 'NONE', #783, #6353 ) ;
#9975 = ORIENTED_EDGE ( 'NONE', *, *, #17385, .T. ) ;
#9976 = CARTESIAN_POINT ( 'NONE',  ( 0.000000000000000000, -1000.000000000000000, -150.0000000000000000 ) ) ;
#9977 = CARTESIAN_POINT ( 'NONE',  ( -64.99999999999998579, -52.79999999999942872, 125.0000000000001421 ) ) ;
#9978 = VERTEX_POINT ( 'NONE', #19657 ) ;
#9979 = CARTESIAN_POINT ( 'NONE',  ( 4.403473400622098133, 6.117907484625861869, 2.043043468777371629E-15 ) ) ;
#9980 = VERTEX_POINT ( 'NONE', #8436 ) ;
#9981 = DIRECTION ( 'NONE',  ( 1.000000000000000000, 0.000000000000000000, 0.000000000000000000 ) ) ;
#9982 = CARTESIAN_POINT ( 'NONE',  ( -20.63749999999999929, 0.000000000000000000, -21.50000000000000000 ) ) ;
#9983 = DIRECTION ( 'NONE',  ( 0.000000000000000000, 0.000000000000000000, 1.000000000000000000 ) ) ;
#9984 = CARTESIAN_POINT ( 'NONE',  ( 2.500000000000000000, -1.178949249685214307, 2.042000000000001592 ) ) ;
#9985 = CIRCLE ( 'NONE', #14238, 0.2000000000000000944 ) ;
#9986 = DIRECTION ( 'NONE',  ( -8.144298233840332611E-17, 0.000000000000000000, -1.000000000000000000 ) ) ;
#9987 = CIRCLE ( 'NONE', #13849, 1.499999999999999556 ) ;
#9988 = CARTESIAN_POINT ( 'NONE',  ( -287.4000000000014552, -127.0000000000000568, 146.4928932188134638 ) ) ;
#9989 = AXIS2_PLACEMENT_3D ( 'NONE', #6876, #10535, #5188 ) ;
#9990 = CARTESIAN_POINT ( 'NONE',  ( 0.000000000000000000, -1000.000000000000000, 90.00000000000000000 ) ) ;
#9991 = VECTOR ( 'NONE', #21436, 1000.000000000000114 ) ;
#9992 = ORIENTED_EDGE ( 'NONE', *, *, #12991, .F. ) ;
#9993 = DIRECTION ( 'NONE',  ( 1.000000000000000000, 0.000000000000000000, 0.000000000000000000 ) ) ;
#9994 = CARTESIAN_POINT ( 'NONE',  ( -146.0000000000005116, -784.4690652294799520, -29.99999999999356604 ) ) ;
#9995 = VERTEX_POINT ( 'NONE', #20902 ) ;
#9996 = ORIENTED_EDGE ( 'NONE', *, *, #15677, .F. ) ;
#9997 = PLANE ( 'NONE',  #1925 ) ;
#9998 = CARTESIAN_POINT ( 'NONE',  ( -44.80746418436648071, -137.9031948627975908, -90.00000000000000000 ) ) ;
#9999 = DIRECTION ( 'NONE',  ( -5.551115123125785858E-15, 5.551115123125785858E-15, -1.000000000000000000 ) ) ;
#10000 = AXIS2_PLACEMENT_3D ( 'NONE', #7048, #7408, #6940 ) ;
#10002 = VECTOR ( 'NONE', #8427, 1000.000000000000000 ) ;
#10001 = PRESENTATION_LAYER_ASSIGNMENT (  '', '', ( #5739 ) ) ;
#10003 = AXIS2_PLACEMENT_3D ( 'NONE', #23633, #22053, #10879 ) ;
#10004 = CARTESIAN_POINT ( 'NONE',  ( 131.5507733270949586, 81.97201125882446604, 29.34395718620175586 ) ) ;
#10005 = VECTOR ( 'NONE', #12770, 1000.000000000000000 ) ;
#10006 = LINE ( 'NONE', #19027, #851 ) ;
#10007 = AXIS2_PLACEMENT_3D ( 'NONE', #9899, #17380, #822 ) ;
#10008 = AXIS2_PLACEMENT_3D ( 'NONE', #10558, #12397, #14178 ) ;
#10009 = LINE ( 'NONE', #2377, #6523 ) ;
#10010 = EDGE_LOOP ( 'NONE', ( #3008, #9244, #16197 ) ) ;
#10011 = DIRECTION ( 'NONE',  ( 0.000000000000000000, -1.000000000000000000, 0.000000000000000000 ) ) ;
#10012 = CARTESIAN_POINT ( 'NONE',  ( 57.99999999999999289, -131.9709811566878273, 2.168404344971008868E-15 ) ) ;
#10013 = AXIS2_PLACEMENT_3D ( 'NONE', #18025, #1357, #6680 ) ;
#10014 =( LENGTH_UNIT ( ) NAMED_UNIT ( * ) SI_UNIT ( .MILLI., .METRE. ) );
#10015 = VERTEX_POINT ( 'NONE', #23164 ) ;
#10016 = CARTESIAN_POINT ( 'NONE',  ( 80.00000000000001421, -56.79999999999998295, 5.199999999999985967 ) ) ;
#10017 = CARTESIAN_POINT ( 'NONE',  ( 0.000000000000000000, 0.000000000000000000, -90.00000000000000000 ) ) ;
#10018 = DIRECTION ( 'NONE',  ( 0.000000000000000000, 0.000000000000000000, 1.000000000000000000 ) ) ;
#10019 = ADVANCED_FACE ( 'NONE', ( #11765 ), #13884, .T. ) ;
#10020 = CARTESIAN_POINT ( 'NONE',  ( 105.0000000000000000, 35.00000000000000000, 0.000000000000000000 ) ) ;
#10021 = UNCERTAINTY_MEASURE_WITH_UNIT (LENGTH_MEASURE( 1.000000000000000082E-05 ), #21885, 'distance_accuracy_value', 'NONE');
#10022 = EDGE_LOOP ( 'NONE', ( #6641, #8814, #8014, #14147 ) ) ;
#10023 = VECTOR ( 'NONE', #893, 1000.000000000000000 ) ;
#10024 = VECTOR ( 'NONE', #7151, 1000.000000000000000 ) ;
#10025 = ORIENTED_EDGE ( 'NONE', *, *, #6648, .F. ) ;
#10027 = AXIS2_PLACEMENT_3D ( 'NONE', #18979, #2562, #4379 ) ;
#10026 = COLOUR_RGB ( '',1.000000000000000000, 0.9490196078431372140, 0.9098039215686274384 ) ;
#10028 = CARTESIAN_POINT ( 'NONE',  ( 0.2500000000000002220, 0.000000000000000000, 0.000000000000000000 ) ) ;
#10029 = AXIS2_PLACEMENT_3D ( 'NONE', #555, #445, #13390 ) ;
#10030 = CARTESIAN_POINT ( 'NONE',  ( -129.2206655591605511, -1072.408698320350595, 30.00000000000641620 ) ) ;
#10031 = AXIS2_PLACEMENT_3D ( 'NONE', #17930, #1149, #21782 ) ;
#10032 = AXIS2_PLACEMENT_3D ( 'NONE', #5919, #2413, #498 ) ;
#10033 = VERTEX_POINT ( 'NONE', #4359 ) ;
#10034 = AXIS2_PLACEMENT_3D ( 'NONE', #1604, #9346, #18036 ) ;
#10035 = AXIS2_PLACEMENT_3D ( 'NONE', #15320, #918, #812 ) ;
#10036 = EDGE_CURVE ( 'NONE', #10801, #6583, #17603, .T. ) ;
#10037 = EDGE_CURVE ( 'NONE', #7103, #14572, #6627, .T. ) ;
#10038 = ORIENTED_EDGE ( 'NONE', *, *, #3626, .F. ) ;
#10039 = CARTESIAN_POINT ( 'NONE',  ( -137.9031948627971076, -44.80746418436799416, -90.00000000000000000 ) ) ;
#10040 = DIRECTION ( 'NONE',  ( 0.000000000000000000, 0.000000000000000000, 1.000000000000000000 ) ) ;
#10041 = ORIENTED_EDGE ( 'NONE', *, *, #11891, .T. ) ;
#10042 = DIRECTION ( 'NONE',  ( 4.625929269271474081E-16, 0.000000000000000000, -1.000000000000000000 ) ) ;
#10043 = EDGE_CURVE ( 'NONE', #10742, #9953, #21467, .T. ) ;
#10044 = ORIENTED_EDGE ( 'NONE', *, *, #2023, .T. ) ;
#10046 = AXIS2_PLACEMENT_3D ( 'NONE', #3293, #18349, #16676 ) ;
#10045 = AXIS2_PLACEMENT_3D ( 'NONE', #10195, #18983, #646 ) ;
#10047 = PLANE ( 'NONE',  #14130 ) ;
#10049 = AXIS2_PLACEMENT_3D ( 'NONE', #10311, #17655, #12270 ) ;
#10048 = CARTESIAN_POINT ( 'NONE',  ( 2.500000000000002220, -1.768423874527823347, 1.021000000000001018 ) ) ;
#10050 = ORIENTED_EDGE ( 'NONE', *, *, #23674, .F. ) ;
#10051 = VERTEX_POINT ( 'NONE', #10517 ) ;
#10052 = CARTESIAN_POINT ( 'NONE',  ( 4.197393957002303999, 7.772902908466098641E-14, -3.503767560748929810 ) ) ;
#10053 = VECTOR ( 'NONE', #7022, 1000.000000000000000 ) ;
#10054 = CIRCLE ( 'NONE', #23527, 2.100000000000000089 ) ;
#10055 = CARTESIAN_POINT ( 'NONE',  ( 45.24999999999994316, 100.0000000000000000, 150.2000000000009550 ) ) ;
#10056 = PLANE ( 'NONE',  #10032 ) ;
#10057 = DIRECTION ( 'NONE',  ( 1.110223024625157172E-14, 0.000000000000000000, -1.000000000000000000 ) ) ;
#10058 = ORIENTED_EDGE ( 'NONE', *, *, #11804, .T. ) ;
#10059 = CARTESIAN_POINT ( 'NONE',  ( -1.282512619719133662, -8.391164935524759727, -7.795653906409117262 ) ) ;
#10060 =( NAMED_UNIT ( * ) SI_UNIT ( $, .STERADIAN. ) SOLID_ANGLE_UNIT ( ) );
#10061 = ORIENTED_EDGE ( 'NONE', *, *, #11367, .F. ) ;
#10062 =( GEOMETRIC_REPRESENTATION_CONTEXT ( 3 ) GLOBAL_UNCERTAINTY_ASSIGNED_CONTEXT ( ( #22318 ) ) GLOBAL_UNIT_ASSIGNED_CONTEXT ( ( #3238, #7111, #14155 ) ) REPRESENTATION_CONTEXT ( 'NONE', 'WORKASPACE' ) );
#10063 = AXIS2_PLACEMENT_3D ( 'NONE', #11834, #9510, #7812 ) ;
#10064 = CIRCLE ( 'NONE', #21237, 145.0000000000000284 ) ;
#10065 = VECTOR ( 'NONE', #11587, 1000.000000000000114 ) ;
#10066 = ORIENTED_EDGE ( 'NONE', *, *, #16300, .F. ) ;
#10067 = EDGE_CURVE ( 'NONE', #13198, #11863, #21167, .T. ) ;
#10068 = B_SPLINE_CURVE_WITH_KNOTS ( 'NONE', 3,
 ( #13188, #16757, #18921, #9887, #6255, #15453, #15093, #2380, #17243, #20866, #22657, #22423, #6129, #13295, #5883, #18786, #4318, #22791, #13661, #2251 ),
 .UNSPECIFIED., .F., .F.,
 ( 4, 2, 2, 2, 2, 2, 2, 2, 2, 4 ),
 ( 0.000000000000000000, 0.001035985217005689577, 0.002071970434011379154, 0.003107955651017068298, 0.003625948259519924579, 0.004143940868022780860, 0.005179926085028581026, 0.006215911302034382926, 0.007251896519040183092, 0.008287881736045983258 ),
 .UNSPECIFIED. ) ;
#10069 = DIRECTION ( 'NONE',  ( 1.000000000000000000, 0.000000000000000000, 0.000000000000000000 ) ) ;
#10070 = EDGE_LOOP ( 'NONE', ( #15198, #9903, #10821, #19955 ) ) ;
#10071 = CARTESIAN_POINT ( 'NONE',  ( 0.000000000000000000, 0.000000000000000000, -90.00000000000000000 ) ) ;
#10072 = ADVANCED_FACE ( 'NONE', ( #16048 ), #5413, .F. ) ;
#10073 = CARTESIAN_POINT ( 'NONE',  ( 21.00000000000000355, 0.000000000000000000, 0.000000000000000000 ) ) ;
#10074 = ADVANCED_FACE ( 'NONE', ( #2003 ), #1561, .F. ) ;
#10075 = ORIENTED_EDGE ( 'NONE', *, *, #9571, .F. ) ;
#10076 = CARTESIAN_POINT ( 'NONE',  ( 145.9999999999998295, -209.9999999999996874, 27.94500000000641649 ) ) ;
#10077 = LINE ( 'NONE', #19329, #19448 ) ;
#10078 = ITEM_DEFINED_TRANSFORMATION ( 'NONE', 'NONE', #21233,  #11210 ) ;
#10079 = ORIENTED_EDGE ( 'NONE', *, *, #18935, .T. ) ;
#10080 = EDGE_CURVE ( 'NONE', #10962, #13026, #22285, .T. ) ;
#10081 = EDGE_CURVE ( 'NONE', #18466, #21466, #16641, .T. ) ;
#10082 = CARTESIAN_POINT ( 'NONE',  ( 5.000000000000000888, 0.000000000000000000, 0.000000000000000000 ) ) ;
#10083 = CARTESIAN_POINT ( 'NONE',  ( -85.22886158240795851, -117.3074641843678876, 90.00000000000000000 ) ) ;
#10084 = DIRECTION ( 'NONE',  ( 1.000000000000000000, 0.000000000000000000, 0.000000000000000000 ) ) ;
#10085 = CARTESIAN_POINT ( 'NONE',  ( -129.2206655591605511, -1072.408698320350595, 30.00000000000641620 ) ) ;
#10086 = CARTESIAN_POINT ( 'NONE',  ( 2.500000000000000000, -1.768423874527823791, -1.020999999999998353 ) ) ;
#10087 = VERTEX_POINT ( 'NONE', #12823 ) ;
#10088 = DIRECTION ( 'NONE',  ( -1.000000000000000000, 1.408839003528726857E-14, 6.982962677686266711E-15 ) ) ;
#10089 = PRODUCT_DEFINITION_SHAPE ( 'NONE', 'NONE',  #23819 ) ;
#10091 = VERTEX_POINT ( 'NONE', #11342 ) ;
#10090 = ORIENTED_EDGE ( 'NONE', *, *, #3617, .F. ) ;
#10092 = CARTESIAN_POINT ( 'NONE',  ( 162.9999999999997726, -209.9999999999996874, 30.00000000000653699 ) ) ;
#10093 = CARTESIAN_POINT ( 'NONE',  ( 7.894958282449824338, -1.603399432398892266, -7.593838100136980351 ) ) ;
#10094 = CARTESIAN_POINT ( 'NONE',  ( 137.9031948627967950, 44.80746418436894629, -90.00000000000000000 ) ) ;
#10095 = CARTESIAN_POINT ( 'NONE',  ( 89.00000000000000000, -94.99999999999998579, 3.000000000000000000 ) ) ;
#10096 = DIRECTION ( 'NONE',  ( -0.7071067811865383579, 0.000000000000000000, 0.7071067811865567876 ) ) ;
#10097 = ORIENTED_EDGE ( 'NONE', *, *, #7296, .T. ) ;
#10098 = DIRECTION ( 'NONE',  ( 0.000000000000000000, -0.5000000000000011102, -0.8660254037844379305 ) ) ;
#10099 = CARTESIAN_POINT ( 'NONE',  ( -109.8074641843675749, 85.22886158240835641, -90.00000000000000000 ) ) ;
#10100 = CARTESIAN_POINT ( 'NONE',  ( -280.0000000000000568, 267.7999999999999545, -146.4928932188134354 ) ) ;
#10101 = ORIENTED_EDGE ( 'NONE', *, *, #22, .T. ) ;
#10102 = DIRECTION ( 'NONE',  ( -0.000000000000000000, 0.000000000000000000, -1.000000000000000000 ) ) ;
#10103 = ORIENTED_EDGE ( 'NONE', *, *, #18741, .T. ) ;
#10104 = CYLINDRICAL_SURFACE ( 'NONE', #12757, 2.500000000000000444 ) ;
#10105 = DIRECTION ( 'NONE',  ( -0.000000000000000000, -0.000000000000000000, 1.000000000000000000 ) ) ;
#10106 = EDGE_CURVE ( 'NONE', #11847, #16299, #20125, .T. ) ;
#10107 = ORIENTED_EDGE ( 'NONE', *, *, #18465, .F. ) ;
#10108 = ADVANCED_FACE ( 'NONE', ( #14481 ), #5762, .F. ) ;
#10109 = LINE ( 'NONE', #18890, #21377 ) ;
#10110 = ORIENTED_EDGE ( 'NONE', *, *, #2973, .T. ) ;
#10111 = CARTESIAN_POINT ( 'NONE',  ( -3.000000000000002665, 0.000000000000000000, 0.000000000000000000 ) ) ;
#10112 = CARTESIAN_POINT ( 'NONE',  ( 279.9999999999999432, 267.7999999999999545, 147.1999999999999886 ) ) ;
#10113 = CARTESIAN_POINT ( 'NONE',  ( -4.000000000000000000, 0.000000000000000000, 0.000000000000000000 ) ) ;
#10114 = CARTESIAN_POINT ( 'NONE',  ( 45.00000000000004974, -56.79999999999967741, 47.35000000000020037 ) ) ;
#10115 = DIRECTION ( 'NONE',  ( -1.000000000000000000, 1.408839003528726857E-14, 6.982962677686266711E-15 ) ) ;
#10116 = VERTEX_POINT ( 'NONE', #5639 ) ;
#10117 = FILL_AREA_STYLE_COLOUR ( '', #15034 ) ;
#10118 = DIRECTION ( 'NONE',  ( -0.7071067811865364705, 0.000000000000000000, 0.7071067811865584529 ) ) ;
#10119 = DIRECTION ( 'NONE',  ( -1.000000000000000000, 0.000000000000000000, 0.000000000000000000 ) ) ;
#10120 = VERTEX_POINT ( 'NONE', #21818 ) ;
#10121 = EDGE_LOOP ( 'NONE', ( #9700, #10167 ) ) ;
#10122 = LINE ( 'NONE', #19615, #1115 ) ;
#10123 = CARTESIAN_POINT ( 'NONE',  ( -158.1195828810602109, 116.4077317428687621, -29.99999999999322498 ) ) ;
#10124 = DIRECTION ( 'NONE',  ( -1.110223024625155594E-14, 0.000000000000000000, -1.000000000000000000 ) ) ;
#10125 = CARTESIAN_POINT ( 'NONE',  ( 2.500000000000002220, 0.000000000000000000, 0.000000000000000000 ) ) ;
#10126 = CARTESIAN_POINT ( 'NONE',  ( 155.0000000000000568, -560.0000000000000000, -60.00000000000000711 ) ) ;
#10127 = SHAPE_REPRESENTATION ( 'MAS-186', ( #13945, #7714, #16204, #2693, #18490, #12001, #1903, #16575, #19266, #17363, #22351, #12383, #4215, #5379, #5787, #1538, #17725, #21957, #21213, #23520, #20416, #10045, #12756, #8101, #12777, #7304, #759, #8880, #21596, #23107, #10829, #8472, #393, #15442, #11206, #13925, #643, #13146, #14294, #20803, #11593, #3464, #16968, #13537, #3836, #2281, #3061, #6156, #20044, #15811, #1136, #14653, #19647, #9253, #22729, #21972, #11, #15832, #17379, #17748, #12020, #774, #14671, #21612, #22750, #22368, #18877, #6958, #7327, #7731, #410, #18507, #5801, #12798, #3482, #13559, #16594, #16996, #13171, #14309, #23152, #15850, #4645, #18143, #20436, #3083, #11230, #21233, #10850 ), #10062 ) ;
#10128 = CARTESIAN_POINT ( 'NONE',  ( 155.0000000000000284, -500.0000000000000000, 27.50000000000001066 ) ) ;
#10129 = ORIENTED_EDGE ( 'NONE', *, *, #7713, .T. ) ;
#10130 = CARTESIAN_POINT ( 'NONE',  ( 158.0000000000000284, -489.9999999999998863, 57.00000000000002132 ) ) ;
#10131 = DIRECTION ( 'NONE',  ( -0.000000000000000000, -1.000000000000000000, -0.000000000000000000 ) ) ;
#10132 = EDGE_CURVE ( 'NONE', #885, #19341, #9035, .T. ) ;
#10133 = DIRECTION ( 'NONE',  ( 1.000000000000000000, 0.000000000000000000, 0.000000000000000000 ) ) ;
#10134 = ORIENTED_EDGE ( 'NONE', *, *, #15976, .T. ) ;
#10135 = CARTESIAN_POINT ( 'NONE',  ( 279.9999999999999432, 272.9999999999999432, 145.0000000000000284 ) ) ;
#10136 = ITEM_DEFINED_TRANSFORMATION ( 'NONE', 'NONE', #17363,  #11210 ) ;
#10137 = ADVANCED_FACE ( 'NONE', ( #14834 ), #7199, .T. ) ;
#10138 = DIRECTION ( 'NONE',  ( -1.000000000000000000, 1.408839003528726857E-14, 6.982962677686266711E-15 ) ) ;
#10139 = CARTESIAN_POINT ( 'NONE',  ( 89.00000000000000000, -94.99999999999998579, 3.000000000000000000 ) ) ;
#10140 = CARTESIAN_POINT ( 'NONE',  ( 135.4018704341550574, 51.87806360044960741, -90.00000000000000000 ) ) ;
#10141 = ORIENTED_EDGE ( 'NONE', *, *, #2891, .F. ) ;
#10142 = EDGE_LOOP ( 'NONE', ( #20301, #18301, #23337, #9776 ) ) ;
#10143 = DIRECTION ( 'NONE',  ( 0.000000000000000000, 0.000000000000000000, -1.000000000000000000 ) ) ;
#10144 = LINE ( 'NONE', #12106, #16210 ) ;
#10145 = VERTEX_POINT ( 'NONE', #3570 ) ;
#10146 = ORIENTED_EDGE ( 'NONE', *, *, #14638, .F. ) ;
#10147 = CARTESIAN_POINT ( 'NONE',  ( 10.12668159690567649, 0.000000000000000000, -9.226681596905677907 ) ) ;
#10148 = LINE ( 'NONE', #8684, #2189 ) ;
#10149 = ORIENTED_EDGE ( 'NONE', *, *, #4891, .F. ) ;
#10150 = CARTESIAN_POINT ( 'NONE',  ( 67.35000000000002274, -87.33333333333332860, 3.000000000000000000 ) ) ;
#10151 = EDGE_CURVE ( 'NONE', #15299, #2147, #21932, .T. ) ;
#10152 = CONICAL_SURFACE ( 'NONE', #9772, 4.000000000000000000, 0.8911886515913786111 ) ;
#10153 = EDGE_LOOP ( 'NONE', ( #19544, #18683, #22892, #22766 ) ) ;
#10154 = EDGE_CURVE ( 'NONE', #5006, #21142, #7337, .T. ) ;
#10155 = CARTESIAN_POINT ( 'NONE',  ( 65.00000000000004263, -52.79999999999959925, 65.00000000000018474 ) ) ;
#10156 = CARTESIAN_POINT ( 'NONE',  ( 0.000000000000000000, 0.000000000000000000, -90.00000000000000000 ) ) ;
#10157 = ORIENTED_EDGE ( 'NONE', *, *, #21474, .F. ) ;
#10158 = ORIENTED_EDGE ( 'NONE', *, *, #9485, .T. ) ;
#10159 = CARTESIAN_POINT ( 'NONE',  ( 4.336808689942017736E-16, 8.660254037844390851, -1.000000000000000888 ) ) ;
#10160 = CARTESIAN_POINT ( 'NONE',  ( 0.000000000000000000, 0.000000000000000000, -25.03750572909317285 ) ) ;
#10161 = FACE_OUTER_BOUND ( 'NONE', #10432, .T. ) ;
#10162 = ORIENTED_EDGE ( 'NONE', *, *, #1758, .T. ) ;
#10163 = DIRECTION ( 'NONE',  ( -1.000000000000000000, -0.000000000000000000, -0.000000000000000000 ) ) ;
#10164 = ADVANCED_FACE ( 'NONE', ( #16747 ), #94, .T. ) ;
#10165 = CIRCLE ( 'NONE', #23643, 0.2500000000000002220 ) ;
#10166 = VERTEX_POINT ( 'NONE', #1759 ) ;
#10167 = ORIENTED_EDGE ( 'NONE', *, *, #9179, .T. ) ;
#10168 = CARTESIAN_POINT ( 'NONE',  ( 18.83866108960308949, -16.51660830817425207, -145.0000000000000000 ) ) ;
#10169 = ORIENTED_EDGE ( 'NONE', *, *, #5322, .T. ) ;
#10170 = DIRECTION ( 'NONE',  ( 1.000000000000000000, 0.000000000000000000, -0.000000000000000000 ) ) ;
#10171 = DIRECTION ( 'NONE',  ( 0.000000000000000000, 1.177509268541832635E-16, -1.000000000000000000 ) ) ;
#10172 = CIRCLE ( 'NONE', #181, 2.055000000000001492 ) ;
#10173 = ORIENTED_EDGE ( 'NONE', *, *, #5173, .F. ) ;
#10174 = PRODUCT_DEFINITION_SHAPE ( 'NONE', 'NONE',  #23806 ) ;
#10175 = VECTOR ( 'NONE', #22725, 1000.000000000000114 ) ;
#10176 = CARTESIAN_POINT ( 'NONE',  ( -59.99999999999996447, -62.00000000000001421, 5.199999999999997513 ) ) ;
#10177 = CARTESIAN_POINT ( 'NONE',  ( -25.00000000000001776, 45.00100000000062295, 124.9999999999998579 ) ) ;
#10178 = CONTEXT_DEPENDENT_SHAPE_REPRESENTATION ( #16774, #12626 ) ;
#10179 = ORIENTED_EDGE ( 'NONE', *, *, #4490, .F. ) ;
#10180 = ADVANCED_FACE ( 'NONE', ( #22165 ), #3687, .T. ) ;
#10181 = CARTESIAN_POINT ( 'NONE',  ( 281.4928932188133786, -127.0000000000000568, 150.2000000000013813 ) ) ;
#10182 = ADVANCED_FACE ( 'NONE', ( #8932 ), #15015, .F. ) ;
#10183 = DIRECTION ( 'NONE',  ( 0.000000000000000000, 0.000000000000000000, 1.000000000000000000 ) ) ;
#10184 = CARTESIAN_POINT ( 'NONE',  ( -102.3500000000000369, 30.00000000000001421, 0.000000000000000000 ) ) ;
#10185 = DIRECTION ( 'NONE',  ( 0.6964005597823107463, -0.7176533009294141507, 6.982962677686266711E-15 ) ) ;
#10186 = ORIENTED_EDGE ( 'NONE', *, *, #2900, .T. ) ;
#10187 = CARTESIAN_POINT ( 'NONE',  ( 2.699999999999995737, 0.000000000000000000, 0.000000000000000000 ) ) ;
#10188 = SURFACE_STYLE_FILL_AREA ( #12046 ) ;
#10189 = EDGE_CURVE ( 'NONE', #1996, #11847, #12337, .T. ) ;
#10190 = CIRCLE ( 'NONE', #19417, 7.499999999999998224 ) ;
#10191 = ADVANCED_FACE ( 'NONE', ( #2238, #2369, #2488 ), #456, .T. ) ;
#10193 = ORIENTED_EDGE ( 'NONE', *, *, #20975, .F. ) ;
#10192 = ORIENTED_EDGE ( 'NONE', *, *, #1652, .F. ) ;
#10194 = AXIS2_PLACEMENT_3D ( 'NONE', #17719, #4092, #18820 ) ;
#10195 = CARTESIAN_POINT ( 'NONE',  ( -135.1560209582351888, 94.48200886273139076, -29.99999999999344880 ) ) ;
#10196 = LINE ( 'NONE', #12051, #16208 ) ;
#10197 = FACE_OUTER_BOUND ( 'NONE', #5675, .T. ) ;
#10198 = PLANE ( 'NONE',  #5753 ) ;
#10199 = CARTESIAN_POINT ( 'NONE',  ( -285.2000000000000455, 267.7999999999999545, -146.4928932188134354 ) ) ;
#10200 = CARTESIAN_POINT ( 'NONE',  ( -146.0000000000000853, -784.4690652294805204, 30.00000000000641620 ) ) ;
#10201 = ORIENTED_EDGE ( 'NONE', *, *, #13734, .T. ) ;
#10202 = CARTESIAN_POINT ( 'NONE',  ( 2.500000000000000000, -1.178949249685214307, 2.042000000000001592 ) ) ;
#10203 = CARTESIAN_POINT ( 'NONE',  ( -137.9031948627974486, 44.80746418436699940, 90.00000000000000000 ) ) ;
#10204 = CARTESIAN_POINT ( 'NONE',  ( 24.99999999999998224, -1000.000000000000000, 145.0000119999999697 ) ) ;
#10205 = CONTEXT_DEPENDENT_SHAPE_REPRESENTATION ( #133, #17192 ) ;
#10206 = ORIENTED_EDGE ( 'NONE', *, *, #12128, .T. ) ;
#10208 = DIRECTION ( 'NONE',  ( 1.110223024625157172E-14, 0.000000000000000000, -1.000000000000000000 ) ) ;
#10207 = CIRCLE ( 'NONE', #18267, 2.649999999999985700 ) ;
#10209 = VERTEX_POINT ( 'NONE', #20716 ) ;
#10210 = CARTESIAN_POINT ( 'NONE',  ( 0.000000000000000000, 0.000000000000000000, -25.03750572909317285 ) ) ;
#10211 = CIRCLE ( 'NONE', #12949, 20.00000000000001776 ) ;
#10212 = DIRECTION ( 'NONE',  ( 0.000000000000000000, 0.000000000000000000, 1.000000000000000000 ) ) ;
#10213 = ORIENTED_EDGE ( 'NONE', *, *, #21281, .F. ) ;
#10214 = CARTESIAN_POINT ( 'NONE',  ( 6.288404560131952259, 5.029641972278931839, -0.4504974108211943773 ) ) ;
#10215 = TOROIDAL_SURFACE ( 'NONE', #17516, 2.700000000000000622, 0.2000000000000000111 ) ;
#10216 = DIRECTION ( 'NONE',  ( 0.000000000000000000, 0.000000000000000000, -1.000000000000000000 ) ) ;
#10217 = CARTESIAN_POINT ( 'NONE',  ( -135.4018704341554269, -51.87806360044865528, 90.00000000000000000 ) ) ;
#10218 = ADVANCED_FACE ( 'NONE', ( #567 ), #2120, .F. ) ;
#10219 = CARTESIAN_POINT ( 'NONE',  ( 145.0000000000000568, -1000.000000000000000, 90.00000000000000000 ) ) ;
#10220 = CARTESIAN_POINT ( 'NONE',  ( -3.510273485745307287, -2.827716139362669967, -3.610536846335890004 ) ) ;
#10221 = EDGE_CURVE ( 'NONE', #15468, #11003, #22780, .T. ) ;
#10222 = DIRECTION ( 'NONE',  ( -1.000000000000000000, -0.000000000000000000, -0.000000000000000000 ) ) ;
#10223 = EDGE_CURVE ( 'NONE', #7547, #10771, #4310, .T. ) ;
#10224 = ORIENTED_EDGE ( 'NONE', *, *, #14365, .F. ) ;
#10225 = SURFACE_SIDE_STYLE ('',( #12607 ) ) ;
#10226 = EDGE_CURVE ( 'NONE', #4142, #13580, #23474, .T. ) ;
#10227 = FACE_OUTER_BOUND ( 'NONE', #13103, .T. ) ;
#10228 = CYLINDRICAL_SURFACE ( 'NONE', #1165, 145.0000000000000284 ) ;
#10229 = EDGE_LOOP ( 'NONE', ( #9231, #20878, #2000 ) ) ;
#10230 = EDGE_LOOP ( 'NONE', ( #14059, #10656, #10276, #17872 ) ) ;
#10231 = DIRECTION ( 'NONE',  ( -1.000000000000000000, 0.000000000000000000, 0.000000000000000000 ) ) ;
#10233 = AXIS2_PLACEMENT_3D ( 'NONE', #12805, #16483, #4024 ) ;
#10232 = FACE_OUTER_BOUND ( 'NONE', #12049, .T. ) ;
#10234 = ADVANCED_FACE ( 'NONE', ( #13762 ), #9997, .F. ) ;
#10235 = ADVANCED_FACE ( 'NONE', ( #21083 ), #5995, .T. ) ;
#10236 = LINE ( 'NONE', #22783, #5205 ) ;
#10237 = AXIS2_PLACEMENT_3D ( 'NONE', #10177, #17521, #12391 ) ;
#10238 = CIRCLE ( 'NONE', #16393, 2.200000000000028155 ) ;
#10239 = DIRECTION ( 'NONE',  ( -1.000000000000000000, -3.469446951953614682E-16, -0.000000000000000000 ) ) ;
#10240 = DIRECTION ( 'NONE',  ( 0.000000000000000000, 0.000000000000000000, 1.000000000000000000 ) ) ;
#10241 = CARTESIAN_POINT ( 'NONE',  ( -2.855764796983342624, 2.970025579236414082, -0.09382832055445475272 ) ) ;
#10242 = ORIENTED_EDGE ( 'NONE', *, *, #13825, .F. ) ;
#10243 = LINE ( 'NONE', #17584, #2892 ) ;
#10244 = DIRECTION ( 'NONE',  ( 1.000000000000000000, 0.000000000000000000, 0.000000000000000000 ) ) ;
#10245 = VECTOR ( 'NONE', #8545, 1000.000000000000000 ) ;
#10246 = PLANE ( 'NONE',  #11375 ) ;
#10247 = ORIENTED_EDGE ( 'NONE', *, *, #8935, .T. ) ;
#10248 = CARTESIAN_POINT ( 'NONE',  ( 100.0000000000000000, -1400.000000000000000, 124.9999999999998295 ) ) ;
#10250 = VECTOR ( 'NONE', #10755, 1000.000000000000000 ) ;
#10249 = CARTESIAN_POINT ( 'NONE',  ( -155.0000000000000284, 0.000000000000000000, 90.00000000000000000 ) ) ;
#10251 = EDGE_CURVE ( 'NONE', #18989, #19049, #5033, .T. ) ;
#10252 = DIRECTION ( 'NONE',  ( 0.000000000000000000, 0.000000000000000000, 1.000000000000000000 ) ) ;
#10253 = CARTESIAN_POINT ( 'NONE',  ( -1.641270926519074580, -1025.000000000000227, -145.0000000000001137 ) ) ;
#10254 = CARTESIAN_POINT ( 'NONE',  ( 105.0000000000000000, 35.00000000000000000, 3.000000000000001332 ) ) ;
#10255 = CARTESIAN_POINT ( 'NONE',  ( -283.5570580646227086, 271.5968359015654983, 145.7154581756739162 ) ) ;
#10256 = CIRCLE ( 'NONE', #11420, 8.000000000000000000 ) ;
#10257 = CLOSED_SHELL ( 'NONE', ( #10108, #5194, #7657, #1300, #4262, #5214, #20037, #18323, #22532, #16075, #21922, #18041, #15241, #18252, #8585, #21111, #13905, #4548, #20429, #15090, #7074, #22038, #12808, #8745, #9480, #23751, #15142, #19893, #14465, #2663, #18500, #5462, #10318, #10263, #23026, #23300, #15184, #22878, #21681, #8358, #17281, #3331, #1977, #4075, #15415, #16429, #4790, #12030, #16980, #22445, #9290, #11245, #427, #13163, #9672, #13972, #7370, #15855, #4115, #9109, #18355, #14508, #22752 ) ) ;
#10258 = VERTEX_POINT ( 'NONE', #17361 ) ;
#10259 = ORIENTED_EDGE ( 'NONE', *, *, #12978, .F. ) ;
#10260 = FACE_OUTER_BOUND ( 'NONE', #22577, .T. ) ;
#10261 = DIRECTION ( 'NONE',  ( 0.000000000000000000, 1.000000000000000000, -1.103561164596346103E-15 ) ) ;
#10262 = ORIENTED_EDGE ( 'NONE', *, *, #22838, .T. ) ;
#10263 = ADVANCED_FACE ( 'NONE', ( #18652, #8184 ), #15193, .F. ) ;
#10264 = CIRCLE ( 'NONE', #23726, 20.00000000000000000 ) ;
#10265 = ADVANCED_FACE ( 'NONE', ( #7687 ), #19141, .F. ) ;
#10266 = ORIENTED_EDGE ( 'NONE', *, *, #14978, .F. ) ;
#10267 = CARTESIAN_POINT ( 'NONE',  ( -56.99999999999995737, -56.79999999999979821, 73.75676759431466678 ) ) ;
#10268 = CARTESIAN_POINT ( 'NONE',  ( -126.5033273815586199, 89.56511165728051083, 30.65186413114638242 ) ) ;
#10269 = CIRCLE ( 'NONE', #23731, 2.649999999999985700 ) ;
#10270 = EDGE_LOOP ( 'NONE', ( #16950, #1744, #7137, #6851 ) ) ;
#10271 = CARTESIAN_POINT ( 'NONE',  ( 2.500000000000002220, -1.178949249685215417, 2.042000000000002036 ) ) ;
#10272 = VECTOR ( 'NONE', #23697, 1000.000000000000000 ) ;
#10273 = ORIENTED_EDGE ( 'NONE', *, *, #3119, .F. ) ;
#10274 = DIRECTION ( 'NONE',  ( 0.000000000000000000, -1.000000000000000000, 0.000000000000000000 ) ) ;
#10275 = CARTESIAN_POINT ( 'NONE',  ( -100.0000000000000000, 249.9999999999999716, 145.0000000000000284 ) ) ;
#10276 = ORIENTED_EDGE ( 'NONE', *, *, #2208, .T. ) ;
#10277 = ORIENTED_EDGE ( 'NONE', *, *, #4107, .T. ) ;
#10278 = DIRECTION ( 'NONE',  ( 0.000000000000000000, 0.000000000000000000, 1.000000000000000000 ) ) ;
#10279 = PRODUCT_DEFINITION_SHAPE ( 'NONE', 'NONE',  #23880 ) ;
#10280 = FACE_OUTER_BOUND ( 'NONE', #10782, .T. ) ;
#10281 = AXIS2_PLACEMENT_3D ( 'NONE', #7171, #12547, #3656 ) ;
#10282 = DIRECTION ( 'NONE',  ( 0.000000000000000000, 1.000000000000000000, -1.295896757998781966E-15 ) ) ;
#10283 = CARTESIAN_POINT ( 'NONE',  ( 0.000000000000000000, 0.000000000000000000, 0.000000000000000000 ) ) ;
#10284 = VERTEX_POINT ( 'NONE', #13283 ) ;
#10285 = CARTESIAN_POINT ( 'NONE',  ( 158.0000000000000284, 4.385380947269369124E-15, 0.000000000000000000 ) ) ;
#10286 =( LENGTH_UNIT ( ) NAMED_UNIT ( * ) SI_UNIT ( .MILLI., .METRE. ) );
#10287 = VERTEX_POINT ( 'NONE', #15558 ) ;
#10288 = ORIENTED_EDGE ( 'NONE', *, *, #6927, .F. ) ;
#10289 = CARTESIAN_POINT ( 'NONE',  ( 1.641270926519074136, -24.99999999999991118, -145.0000000000000000 ) ) ;
#10290 = ORIENTED_EDGE ( 'NONE', *, *, #21312, .F. ) ;
#10291 = CIRCLE ( 'NONE', #6813, 21.50000000000000000 ) ;
#10292 = LINE ( 'NONE', #8831, #7150 ) ;
#10293 = FACE_BOUND ( 'NONE', #7775, .T. ) ;
#10294 = ORIENTED_EDGE ( 'NONE', *, *, #18856, .F. ) ;
#10295 = AXIS2_PLACEMENT_3D ( 'NONE', #19978, #1394, #14454 ) ;
#10296 = CARTESIAN_POINT ( 'NONE',  ( -155.0000000000000284, -204.4690652294806057, 30.00000000000648015 ) ) ;
#10297 = CARTESIAN_POINT ( 'NONE',  ( 121.5574576620388143, 79.04925354955381067, -2.775557561562891351E-14 ) ) ;
#10298 = ITEM_DEFINED_TRANSFORMATION ( 'NONE', 'NONE', #10850,  #11210 ) ;
#10299 = ORIENTED_EDGE ( 'NONE', *, *, #13717, .T. ) ;
#10300 = CARTESIAN_POINT ( 'NONE',  ( 281.4928932188133217, -132.2000000000000455, 152.4000000000014268 ) ) ;
#10301 = DIRECTION ( 'NONE',  ( 1.000000000000000000, 0.000000000000000000, 0.000000000000000000 ) ) ;
#10302 = VECTOR ( 'NONE', #1081, 1000.000000000000000 ) ;
#10303 = DIRECTION ( 'NONE',  ( -0.000000000000000000, 1.000000000000000000, 1.224646799147353207E-16 ) ) ;
#10304 = DIRECTION ( 'NONE',  ( -0.000000000000000000, -0.000000000000000000, 1.000000000000000000 ) ) ;
#10305 = ORIENTED_EDGE ( 'NONE', *, *, #11441, .F. ) ;
#10306 = CARTESIAN_POINT ( 'NONE',  ( 282.2000000000013529, -127.0000000000000568, 146.4928932188134638 ) ) ;
#10307 = AXIS2_PLACEMENT_3D ( 'NONE', #15113, #18573, #11489 ) ;
#10309 = ORIENTED_EDGE ( 'NONE', *, *, #2730, .T. ) ;
#10308 = VERTEX_POINT ( 'NONE', #22884 ) ;
#10310 = CARTESIAN_POINT ( 'NONE',  ( 70.00000000000000000, -112.6666666666666856, 153.0000000000000000 ) ) ;
#10311 = CARTESIAN_POINT ( 'NONE',  ( -129.2206655591605511, -1072.408698320350595, 30.00000000000641620 ) ) ;
#10312 = CARTESIAN_POINT ( 'NONE',  ( 132.1836189744869898, 80.94757571328915446, -32.17188107257626228 ) ) ;
#10313 = DIRECTION ( 'NONE',  ( 1.000000000000000000, 0.000000000000000000, 0.000000000000000000 ) ) ;
#10314 = DIRECTION ( 'NONE',  ( 1.000000000000000000, 0.000000000000000000, 0.000000000000000000 ) ) ;
#10315 = EDGE_CURVE ( 'NONE', #8126, #5651, #22371, .T. ) ;
#10316 = CARTESIAN_POINT ( 'NONE',  ( -282.1427398886704054, 268.3758453455903918, -146.2440776823445390 ) ) ;
#10317 = ORIENTED_EDGE ( 'NONE', *, *, #6987, .F. ) ;
#10318 = ADVANCED_FACE ( 'NONE', ( #11590 ), #4048, .T. ) ;
#10319 = ADVANCED_FACE ( 'NONE', ( #9875 ), #6117, .T. ) ;
#10320 = CIRCLE ( 'NONE', #18030, 2.649999999999985700 ) ;
#10321 = FACE_BOUND ( 'NONE', #18423, .T. ) ;
#10322 = EDGE_LOOP ( 'NONE', ( #7505, #857, #13176, #2844 ) ) ;
#10323 = VECTOR ( 'NONE', #13312, 1000.000000000000114 ) ;
#10324 = CARTESIAN_POINT ( 'NONE',  ( 2.500000000000000000, 0.000000000000000000, 0.000000000000000000 ) ) ;
#10325 = CARTESIAN_POINT ( 'NONE',  ( 145.0000000000000284, 1.518794382396763073E-12, 90.00000000000000000 ) ) ;
#10326 = EDGE_CURVE ( 'NONE', #14070, #21880, #16133, .T. ) ;
#10327 = VECTOR ( 'NONE', #4233, 1000.000000000000000 ) ;
#10328 = ITEM_DEFINED_TRANSFORMATION ( 'NONE', 'NONE', #16968,  #11210 ) ;
#10329 = ORIENTED_EDGE ( 'NONE', *, *, #4569, .T. ) ;
#10330 = CARTESIAN_POINT ( 'NONE',  ( -0.5449313310646672903, -4.304185902836978883, -3.316620875263469159 ) ) ;
#10331 = ORIENTED_EDGE ( 'NONE', *, *, #20806, .F. ) ;
#10332 = CARTESIAN_POINT ( 'NONE',  ( -31.74999999999995737, 0.000000000000000000, 0.000000000000000000 ) ) ;
#10333 = DIRECTION ( 'NONE',  ( 1.000000000000000000, 0.000000000000000000, 0.000000000000000000 ) ) ;
#10334 = ORIENTED_EDGE ( 'NONE', *, *, #19326, .T. ) ;
#10335 = DIRECTION ( 'NONE',  ( -1.000000000000000000, -0.000000000000000000, -0.000000000000000000 ) ) ;
#10336 =( NAMED_UNIT ( * ) SI_UNIT ( $, .STERADIAN. ) SOLID_ANGLE_UNIT ( ) );
#10337 = DIRECTION ( 'NONE',  ( -0.6663528160695909586, -0.2365880903936287138, 0.7071067811865631159 ) ) ;
#10338 = CARTESIAN_POINT ( 'NONE',  ( -117.3074641843669781, -85.22886158240918064, -90.00000000000000000 ) ) ;
#10339 = CARTESIAN_POINT ( 'NONE',  ( -194.7500000000000568, -204.4690652294800657, 27.50000000000675371 ) ) ;
#10340 = CARTESIAN_POINT ( 'NONE',  ( 0.5974722283283632196, -8.315303285985693904, -0.7026937717022971874 ) ) ;
#10341 = VECTOR ( 'NONE', #10345, 1000.000000000000000 ) ;
#10342 = CARTESIAN_POINT ( 'NONE',  ( -117.3074641843675749, 85.22886158240835641, -90.00000000000000000 ) ) ;
#10343 = ORIENTED_EDGE ( 'NONE', *, *, #1188, .T. ) ;
#10344 =( LENGTH_UNIT ( ) NAMED_UNIT ( * ) SI_UNIT ( .MILLI., .METRE. ) );
#10345 = DIRECTION ( 'NONE',  ( -0.000000000000000000, -0.000000000000000000, 1.000000000000000000 ) ) ;
#10346 = AXIS2_PLACEMENT_3D ( 'NONE', #15639, #10459, #2708 ) ;
#10347 = DIRECTION ( 'NONE',  ( 1.000000000000000000, 0.000000000000000000, 0.000000000000000000 ) ) ;
#10348 = ORIENTED_EDGE ( 'NONE', *, *, #215, .T. ) ;
#10349 = ORIENTED_EDGE ( 'NONE', *, *, #15251, .T. ) ;
#10350 = CIRCLE ( 'NONE', #12310, 2.055000000000001492 ) ;
#10351 = CARTESIAN_POINT ( 'NONE',  ( -67.34999999999998010, -87.33333333333338544, 3.000000000000001332 ) ) ;
#10352 = DIRECTION ( 'NONE',  ( -0.000000000000000000, -0.000000000000000000, 1.000000000000000000 ) ) ;
#10353 =( REPRESENTATION_RELATIONSHIP ('NONE','NONE', #10127, #18083 ) REPRESENTATION_RELATIONSHIP_WITH_TRANSFORMATION ( #21674 )SHAPE_REPRESENTATION_RELATIONSHIP( ) );
#10354 = LINE ( 'NONE', #17697, #2492 ) ;
#10355 = ADVANCED_FACE ( 'NONE', ( #6470 ), #6825, .F. ) ;
#10356 = CARTESIAN_POINT ( 'NONE',  ( 2.500000000000000000, 0.000000000000000000, 2.041999999999999815 ) ) ;
#10357 = CARTESIAN_POINT ( 'NONE',  ( -284.5135885331259260, 270.4045710003934460, -145.9955614683502176 ) ) ;
#10358 = EDGE_CURVE ( 'NONE', #13805, #327, #17466, .T. ) ;
#10359 = AXIS2_PLACEMENT_3D ( 'NONE', #7167, #21894, #22024 ) ;
#10360 = DIRECTION ( 'NONE',  ( -0.000000000000000000, -0.000000000000000000, 1.000000000000000000 ) ) ;
#10361 = ADVANCED_FACE ( 'NONE', ( #23490 ), #779, .F. ) ;
#10362 = EDGE_LOOP ( 'NONE', ( #7642, #12187, #1337, #11868 ) ) ;
#10363 = LINE ( 'NONE', #17711, #19107 ) ;
#10364 = CARTESIAN_POINT ( 'NONE',  ( 5.000000000000000000, 4.685197434473814759, -5.637851296924623057E-15 ) ) ;
#10365 = AXIS2_PLACEMENT_3D ( 'NONE', #976, #8356, #6551 ) ;
#10366 = CIRCLE ( 'NONE', #15378, 145.0000000000000284 ) ;
#10367 = PLANE ( 'NONE',  #5184 ) ;
#10368 = CIRCLE ( 'NONE', #16912, 2.700000000000000622 ) ;
#10369 = VERTEX_POINT ( 'NONE', #17694 ) ;
#10370 = SURFACE_STYLE_USAGE ( .BOTH. , #2962 ) ;
#10371 = AXIS2_PLACEMENT_3D ( 'NONE', #19976, #20206, #18392 ) ;
#10372 = EDGE_CURVE ( 'NONE', #16588, #1219, #2948, .T. ) ;
#10373 = LINE ( 'NONE', #16277, #17287 ) ;
#10374 = PLANE ( 'NONE',  #23547 ) ;
#10375 = PRODUCT_RELATED_PRODUCT_CATEGORY ( 'part', '', ( #1687 ) ) ;
#10376 = DIRECTION ( 'NONE',  ( 1.350636282998972974E-14, 0.000000000000000000, -1.000000000000000000 ) ) ;
#10377 = CARTESIAN_POINT ( 'NONE',  ( 0.000000000000000000, 11.99999999999999822, 200.0000000000000000 ) ) ;
#10378 = FACE_OUTER_BOUND ( 'NONE', #19062, .T. ) ;
#10379 = CARTESIAN_POINT ( 'NONE',  ( -144.8060344827586050, -7.497491405672224829, 90.00000000000000000 ) ) ;
#10380 = VERTEX_POINT ( 'NONE', #10351 ) ;
#10381 = EDGE_LOOP ( 'NONE', ( #19184, #6446 ) ) ;
#10382 = CARTESIAN_POINT ( 'NONE',  ( -280.8703180930666576, 269.1429506979392272, -146.7484459290826067 ) ) ;
#10383 = DIRECTION ( 'NONE',  ( 1.000000000000000000, 0.000000000000000000, -0.000000000000000000 ) ) ;
#10384 = EDGE_LOOP ( 'NONE', ( #8450, #23425, #7391, #18815 ) ) ;
#10385 = PRODUCT ( 'socket head cap screw_iso_ISO 4762 M5 x 30 - 22N', 'socket head cap screw_iso_ISO 4762 M5 x 30 - 22N', '', ( #20143 ) ) ;
#10386 = DIRECTION ( 'NONE',  ( -1.000000000000000000, 0.000000000000000000, 0.000000000000000000 ) ) ;
#10387 = LINE ( 'NONE', #8121, #3760 ) ;
#10388 = CIRCLE ( 'NONE', #14615, 2.041999999999999815 ) ;
#10389 = CIRCLE ( 'NONE', #19606, 145.0000000000000284 ) ;
#10390 = ORIENTED_EDGE ( 'NONE', *, *, #7871, .F. ) ;
#10391 = CARTESIAN_POINT ( 'NONE',  ( 90.00000000000000000, 95.00000000000000000, 3.000000000000000000 ) ) ;
#10392 = CIRCLE ( 'NONE', #9597, 145.0000000000000284 ) ;
#10393 = CARTESIAN_POINT ( 'NONE',  ( 281.4928932188133217, -127.0000000000000568, 147.2000000000014381 ) ) ;
#10394 = ORIENTED_EDGE ( 'NONE', *, *, #13421, .T. ) ;
#10395 = CARTESIAN_POINT ( 'NONE',  ( -134.8087563975455225, -1076.495802945233663, -28.46728581292316207 ) ) ;
#10396 = AXIS2_PLACEMENT_3D ( 'NONE', #18215, #14169, #3830 ) ;
#10397 = ORIENTED_EDGE ( 'NONE', *, *, #14082, .T. ) ;
#10398 = CARTESIAN_POINT ( 'NONE',  ( -85.22886158240795851, -117.3074641843678876, -90.00000000000000000 ) ) ;
#10399 = DIRECTION ( 'NONE',  ( 0.000000000000000000, 0.000000000000000000, -1.000000000000000000 ) ) ;
#10400 = EDGE_LOOP ( 'NONE', ( #5841, #6840, #19538, #19999 ) ) ;
#10401 = ORIENTED_EDGE ( 'NONE', *, *, #9813, .F. ) ;
#10402 = CARTESIAN_POINT ( 'NONE',  ( 133.9969223633123079, 77.90910650221316303, -28.88783501520648400 ) ) ;
#10403 = APPLICATION_PROTOCOL_DEFINITION ( 'draft international standard', 'automotive_design', 1998, #20150 ) ;
#10404 = CIRCLE ( 'NONE', #16188, 7.500000000000003553 ) ;
#10405 = LINE ( 'NONE', #842, #12022 ) ;
#10406 = EDGE_CURVE ( 'NONE', #15945, #16256, #11954, .T. ) ;
#10407 = EDGE_CURVE ( 'NONE', #9902, #829, #21210, .T. ) ;
#10408 = VECTOR ( 'NONE', #21861, 1000.000000000000000 ) ;
#10409 = CIRCLE ( 'NONE', #17702, 0.2000000000000000944 ) ;
#10410 = AXIS2_PLACEMENT_3D ( 'NONE', #13525, #5862, #18639 ) ;
#10411 = EDGE_CURVE ( 'NONE', #11870, #3113, #12440, .T. ) ;
#10413 = CARTESIAN_POINT ( 'NONE',  ( -2.325424218463065351, 7.317669739334662360, -7.030005583190789054 ) ) ;
#10412 = AXIS2_PLACEMENT_3D ( 'NONE', #16124, #10592, #16010 ) ;
#10414 = FACE_OUTER_BOUND ( 'NONE', #3578, .T. ) ;
#10415 = EDGE_LOOP ( 'NONE', ( #15618, #19365, #13680, #9474 ) ) ;
#10416 = LINE ( 'NONE', #8584, #8355 ) ;
#10417 = FILL_AREA_STYLE_COLOUR ( '', #21165 ) ;
#10418 = VERTEX_POINT ( 'NONE', #4671 ) ;
#10419 = VECTOR ( 'NONE', #155, 1000.000000000000000 ) ;
#10420 = CARTESIAN_POINT ( 'NONE',  ( 70.00000000000000000, -112.6666666666666714, 144.9999999999999716 ) ) ;
#10421 = CARTESIAN_POINT ( 'NONE',  ( 0.000000000000000000, 0.000000000000000000, 0.000000000000000000 ) ) ;
#10423 = AXIS2_PLACEMENT_3D ( 'NONE', #23346, #13631, #13859 ) ;
#10422 = AXIS2_PLACEMENT_3D ( 'NONE', #14917, #20095, #16959 ) ;
#10424 = ORIENTED_EDGE ( 'NONE', *, *, #22935, .F. ) ;
#10425 = CARTESIAN_POINT ( 'NONE',  ( 6.658902113225075858, 5.287118297641098863, -7.776713651267108673 ) ) ;
#10426 = CIRCLE ( 'NONE', #17729, 2.500000000000002220 ) ;
#10427 = AXIS2_PLACEMENT_3D ( 'NONE', #6568, #2915, #10314 ) ;
#10428 = AXIS2_PLACEMENT_3D ( 'NONE', #19440, #4618, #4729 ) ;
#10429 = FACE_BOUND ( 'NONE', #15098, .T. ) ;
#10430 = AXIS2_PLACEMENT_3D ( 'NONE', #3661, #5260, #19979 ) ;
#10431 = AXIS2_PLACEMENT_3D ( 'NONE', #6739, #21464, #4927 ) ;
#10432 = EDGE_LOOP ( 'NONE', ( #190, #10097, #21757, #14535 ) ) ;
#10433 = CIRCLE ( 'NONE', #4226, 2.649999999999992806 ) ;
#10434 = CARTESIAN_POINT ( 'NONE',  ( -136.7455495141628887, -1072.977142426287401, 28.46749050845390983 ) ) ;
#10435 = DIRECTION ( 'NONE',  ( -1.000000000000000000, 3.495664435217746987E-15, 0.000000000000000000 ) ) ;
#10436 = ORIENTED_EDGE ( 'NONE', *, *, #1554, .T. ) ;
#10437 = CARTESIAN_POINT ( 'NONE',  ( -100.0000000000000000, 250.0000000000000000, -124.9999999999999716 ) ) ;
#10438 = FACE_OUTER_BOUND ( 'NONE', #14977, .T. ) ;
#10439 = DIRECTION ( 'NONE',  ( -5.551115123125785858E-15, 5.551115123125785858E-15, -1.000000000000000000 ) ) ;
#10440 = CARTESIAN_POINT ( 'NONE',  ( 45.00000000000000711, 5.510910596163090344E-15, 169.9999999999999716 ) ) ;
#10441 = EDGE_CURVE ( 'NONE', #15992, #14150, #10122, .T. ) ;
#10442 = CARTESIAN_POINT ( 'NONE',  ( 35.00000000000000000, 4.286263797015736496E-15, -100.0000000000000000 ) ) ;
#10443 = VERTEX_POINT ( 'NONE', #17940 ) ;
#10444 = PRODUCT_DEFINITION_FORMATION_WITH_SPECIFIED_SOURCE ( 'ANY', '', #23666, .NOT_KNOWN. ) ;
#10445 = DIRECTION ( 'NONE',  ( -1.000000000000000000, -0.000000000000000000, -0.000000000000000000 ) ) ;
#10446 = FILL_AREA_STYLE_COLOUR ( '', #15835 ) ;
#10447 = AXIS2_PLACEMENT_3D ( 'NONE', #6678, #21398, #3393 ) ;
#10448 = CIRCLE ( 'NONE', #8125, 2.499999999999946709 ) ;
#10449 = AXIS2_PLACEMENT_3D ( 'NONE', #11678, #15159, #18872 ) ;
#10451 = ORIENTED_EDGE ( 'NONE', *, *, #6601, .T. ) ;
#10450 = ORIENTED_EDGE ( 'NONE', *, *, #940, .T. ) ;
#10452 = DIRECTION ( 'NONE',  ( 2.832769448823989808E-16, -1.000000000000000000, 3.469446951953613794E-15 ) ) ;
#10453 = CARTESIAN_POINT ( 'NONE',  ( 7.500000000000000000, 0.7723602884954153813, -7.026388801733942202 ) ) ;
#10454 = DIRECTION ( 'NONE',  ( 1.000000000000000000, 0.000000000000000000, 0.000000000000000000 ) ) ;
#10455 = CARTESIAN_POINT ( 'NONE',  ( 0.000000000000000000, 0.000000000000000000, -50.00000000000000000 ) ) ;
#10456 = FACE_OUTER_BOUND ( 'NONE', #15148, .T. ) ;
#10457 = DIRECTION ( 'NONE',  ( -1.350636282998972974E-14, 0.000000000000000000, -1.000000000000000000 ) ) ;
#10458 = ORIENTED_EDGE ( 'NONE', *, *, #6359, .T. ) ;
#10459 = DIRECTION ( 'NONE',  ( 0.9289202219288174023, 0.3702799228849934510, 6.982962677686266711E-15 ) ) ;
#10460 = ORIENTED_EDGE ( 'NONE', *, *, #20025, .T. ) ;
#10461 = CARTESIAN_POINT ( 'NONE',  ( 282.2000000000013529, -127.0000000000000568, 145.0000000000000284 ) ) ;
#10462 = DIRECTION ( 'NONE',  ( 1.000000000000000000, -0.000000000000000000, 6.982962677686266711E-15 ) ) ;
#10463 = PRESENTATION_STYLE_ASSIGNMENT (( #23220 ) ) ;
#10464 = CONTEXT_DEPENDENT_SHAPE_REPRESENTATION ( #21266, #23572 ) ;
#10465 = EDGE_CURVE ( 'NONE', #3693, #15263, #14630, .T. ) ;
#10466 = EDGE_LOOP ( 'NONE', ( #9336, #10865 ) ) ;
#10467 = DIRECTION ( 'NONE',  ( 0.000000000000000000, 0.000000000000000000, 1.000000000000000000 ) ) ;
#10468 = ORIENTED_EDGE ( 'NONE', *, *, #14644, .F. ) ;
#10469 = LINE ( 'NONE', #4653, #23108 ) ;
#10470 = FACE_OUTER_BOUND ( 'NONE', #19124, .T. ) ;
#10471 = VERTEX_POINT ( 'NONE', #8771 ) ;
#10472 =( NAMED_UNIT ( * ) PLANE_ANGLE_UNIT ( ) SI_UNIT ( $, .RADIAN. ) );
#10473 =( NAMED_UNIT ( * ) PLANE_ANGLE_UNIT ( ) SI_UNIT ( $, .RADIAN. ) );
#10474 = CARTESIAN_POINT ( 'NONE',  ( -79.04925354955248906, 121.5574576620396812, 90.00000000000000000 ) ) ;
#10475 = EDGE_CURVE ( 'NONE', #6640, #9371, #8292, .T. ) ;
#10476 = CARTESIAN_POINT ( 'NONE',  ( 45.24999999999994316, 100.0000000000000000, -125.0000000000000000 ) ) ;
#10477 = DIRECTION ( 'NONE',  ( -1.000000000000000000, 1.408839003528726857E-14, 6.982962677686266711E-15 ) ) ;
#10478 = DIRECTION ( 'NONE',  ( 0.000000000000000000, 0.000000000000000000, -1.000000000000000000 ) ) ;
#10479 = ADVANCED_FACE ( 'NONE', ( #23366 ), #2835, .F. ) ;
#10480 = PLANE ( 'NONE',  #3582 ) ;
#10481 = EDGE_LOOP ( 'NONE', ( #17946, #14753, #23032 ) ) ;
#10482 = DIRECTION ( 'NONE',  ( 1.000000000000000000, 0.000000000000000000, 0.000000000000000000 ) ) ;
#10483 = FACE_OUTER_BOUND ( 'NONE', #158, .T. ) ;
#10484 = EDGE_CURVE ( 'NONE', #12825, #21826, #10409, .T. ) ;
#10485 = ORIENTED_EDGE ( 'NONE', *, *, #1574, .F. ) ;
#10486 = ORIENTED_EDGE ( 'NONE', *, *, #19677, .T. ) ;
#10487 = DIRECTION ( 'NONE',  ( 0.000000000000000000, 0.000000000000000000, -1.000000000000000000 ) ) ;
#10488 = LINE ( 'NONE', #12086, #2635 ) ;
#10490 = CARTESIAN_POINT ( 'NONE',  ( -280.0000000000000568, 269.9696999999999889, 145.0000000000000284 ) ) ;
#10489 = PRODUCT_DEFINITION_SHAPE ( 'NONE', 'NONE',  #23822 ) ;
#10491 = CARTESIAN_POINT ( 'NONE',  ( 132.8404720734530144, 79.86494211668949106, 27.50000000000646239 ) ) ;
#10492 = CARTESIAN_POINT ( 'NONE',  ( 17.00000000000000000, 0.000000000000000000, 0.000000000000000000 ) ) ;
#10493 = VERTEX_POINT ( 'NONE', #15668 ) ;
#10494 = DIRECTION ( 'NONE',  ( 0.000000000000000000, -0.5000000000000011102, -0.8660254037844379305 ) ) ;
#10495 = ORIENTED_EDGE ( 'NONE', *, *, #14410, .F. ) ;
#10496 = DIRECTION ( 'NONE',  ( -1.110223024625155594E-14, 0.000000000000000000, -1.000000000000000000 ) ) ;
#10497 = CARTESIAN_POINT ( 'NONE',  ( 160.0000000000000000, 1.959434878635765210E-14, -100.0000000000000000 ) ) ;
#10498 = CYLINDRICAL_SURFACE ( 'NONE', #19041, 2.500000000000000444 ) ;
#10499 = ORIENTED_EDGE ( 'NONE', *, *, #16521, .F. ) ;
#10500 = DIRECTION ( 'NONE',  ( 1.000000000000000000, 0.000000000000000000, 0.000000000000000000 ) ) ;
#10501 =( REPRESENTATION_RELATIONSHIP ('NONE','NONE', #10127, #18083 ) REPRESENTATION_RELATIONSHIP_WITH_TRANSFORMATION ( #18995 )SHAPE_REPRESENTATION_RELATIONSHIP( ) );
#10502 = FACE_OUTER_BOUND ( 'NONE', #14811, .T. ) ;
#10503 = ADVANCED_FACE ( 'NONE', ( #22997 ), #13998, .T. ) ;
#10504 = DIRECTION ( 'NONE',  ( 0.3090169943749441761, 0.9510565162951546414, 0.000000000000000000 ) ) ;
#10505 = CYLINDRICAL_SURFACE ( 'NONE', #17133, 145.0000000000000284 ) ;
#10506 = EDGE_CURVE ( 'NONE', #21618, #846, #4778, .T. ) ;
#10507 = DIRECTION ( 'NONE',  ( 0.000000000000000000, 0.000000000000000000, 1.000000000000000000 ) ) ;
#10508 = DIRECTION ( 'NONE',  ( 0.000000000000000000, 0.000000000000000000, -1.000000000000000000 ) ) ;
#10509 = CARTESIAN_POINT ( 'NONE',  ( -284.9324007871372828, 269.4810649015074659, 146.1807969192697954 ) ) ;
#10510 = ORIENTED_EDGE ( 'NONE', *, *, #9712, .T. ) ;
#10511 = ORIENTED_EDGE ( 'NONE', *, *, #23275, .T. ) ;
#10512 = DIRECTION ( 'NONE',  ( -1.000000000000000000, -0.000000000000000000, -0.000000000000000000 ) ) ;
#10513 = CARTESIAN_POINT ( 'NONE',  ( 137.9031948627977044, -44.80746418436605438, -90.00000000000000000 ) ) ;
#10514 = EDGE_CURVE ( 'NONE', #12610, #6490, #6712, .T. ) ;
#10515 = ORIENTED_EDGE ( 'NONE', *, *, #4255, .F. ) ;
#10516 = EDGE_CURVE ( 'NONE', #19505, #15324, #2958, .T. ) ;
#10517 = CARTESIAN_POINT ( 'NONE',  ( 0.000000000000000000, 2.342598717236902939, -4.057500000000001883 ) ) ;
#10518 = FACE_OUTER_BOUND ( 'NONE', #232, .T. ) ;
#10519 = ORIENTED_EDGE ( 'NONE', *, *, #22597, .F. ) ;
#10520 = CYLINDRICAL_SURFACE ( 'NONE', #8709, 4.250000000000000000 ) ;
#10521 = EDGE_CURVE ( 'NONE', #3131, #22831, #14450, .T. ) ;
#10522 = CYLINDRICAL_SURFACE ( 'NONE', #7595, 2.649999999999971934 ) ;
#10523 = EDGE_LOOP ( 'NONE', ( #16756, #12360 ) ) ;
#10524 = CARTESIAN_POINT ( 'NONE',  ( 80.00000000000000000, -59.79999999999998295, 5.199999999999989519 ) ) ;
#10525 = EDGE_CURVE ( 'NONE', #21860, #10369, #13539, .T. ) ;
#10526 = VERTEX_POINT ( 'NONE', #22028 ) ;
#10527 = CARTESIAN_POINT ( 'NONE',  ( 0.000000000000000000, 0.000000000000000000, -90.00000000000000000 ) ) ;
#10528 = CARTESIAN_POINT ( 'NONE',  ( -49.99999999999997158, 1.678138721159888895E-29, 4.479364028612180224E-15 ) ) ;
#10529 = ORIENTED_EDGE ( 'NONE', *, *, #18498, .T. ) ;
#10530 = ORIENTED_EDGE ( 'NONE', *, *, #19418, .F. ) ;
#10531 = CARTESIAN_POINT ( 'NONE',  ( 133.0100681275902730, 79.58233248384551928, -32.48402282453940870 ) ) ;
#10532 = VECTOR ( 'NONE', #18917, 1000.000000000000000 ) ;
#10533 = APPLICATION_PROTOCOL_DEFINITION ( 'draft international standard', 'automotive_design', 1998, #6135 ) ;
#10534 = CARTESIAN_POINT ( 'NONE',  ( -280.6845057130643681, 271.7107452280324082, -148.4314821058792404 ) ) ;
#10535 = DIRECTION ( 'NONE',  ( 1.000000000000000000, -3.495664435217746987E-15, -0.000000000000000000 ) ) ;
#10536 = FACE_OUTER_BOUND ( 'NONE', #10919, .T. ) ;
#10537 = ORIENTED_EDGE ( 'NONE', *, *, #20858, .F. ) ;
#10538 = EDGE_CURVE ( 'NONE', #6623, #2188, #6541, .T. ) ;
#10539 = PLANE ( 'NONE',  #14543 ) ;
#10540 = VERTEX_POINT ( 'NONE', #7530 ) ;
#10541 = B_SPLINE_CURVE_WITH_KNOTS ( 'NONE', 3,
 ( #6671, #14065, #3386, #16330, #23321, #5922, #7489, #13099 ),
 .UNSPECIFIED., .F., .F.,
 ( 4, 2, 2, 4 ),
 ( 0.006061689441712453386, 0.007174127271521677299, 0.008286565101330901212, 0.01051144076094934904 ),
 .UNSPECIFIED. ) ;
#10542 = ADVANCED_FACE ( 'NONE', ( #16474 ), #10848, .F. ) ;
#10543 = VERTEX_POINT ( 'NONE', #21901 ) ;
#10544 = CARTESIAN_POINT ( 'NONE',  ( 24.19933745025248228, -6.487655866515820158, -145.0000000000000000 ) ) ;
#10545 = EDGE_CURVE ( 'NONE', #16945, #15162, #3654, .T. ) ;
#10546 = EDGE_CURVE ( 'NONE', #1647, #22518, #17730, .T. ) ;
#10547 = VERTEX_POINT ( 'NONE', #20100 ) ;
#10549 = EDGE_CURVE ( 'NONE', #2171, #23104, #19626, .T. ) ;
#10548 = DIRECTION ( 'NONE',  ( -1.000000000000000000, 0.000000000000000000, 0.000000000000000000 ) ) ;
#10550 = ORIENTED_EDGE ( 'NONE', *, *, #19223, .T. ) ;
#10551 = B_SPLINE_CURVE_WITH_KNOTS ( 'NONE', 3,
 ( #17676, #4885, #10586, #12072, #19601, #4659 ),
 .UNSPECIFIED., .F., .F.,
 ( 4, 2, 4 ),
 ( 0.004615310220740751271, 0.006918661718823357169, 0.009222013216905963068 ),
 .UNSPECIFIED. ) ;
#10552 = DIRECTION ( 'NONE',  ( 0.9396926207859138680, 1.150791560227856926E-16, -0.3420201433256536139 ) ) ;
#10553 = VERTEX_POINT ( 'NONE', #12900 ) ;
#10554 = LINE ( 'NONE', #4850, #5017 ) ;
#10555 = CARTESIAN_POINT ( 'NONE',  ( 60.00000000000000000, -137.1994082814340743, -2.400000000000046096 ) ) ;
#10556 = AXIS2_PLACEMENT_3D ( 'NONE', #1908, #19913, #1570 ) ;
#10557 = CARTESIAN_POINT ( 'NONE',  ( -37.64999999999999147, 90.00000000000001421, 3.000000000000000000 ) ) ;
#10558 = CARTESIAN_POINT ( 'NONE',  ( 146.4450000000002490, -801.0618695410406644, -29.99999999999356248 ) ) ;
#10559 = VERTEX_POINT ( 'NONE', #10957 ) ;
#10560 = CARTESIAN_POINT ( 'NONE',  ( -146.4450000000000784, -204.4690652294807194, 30.00000000000641975 ) ) ;
#10562 = ORIENTED_EDGE ( 'NONE', *, *, #18293, .T. ) ;
#10561 = ORIENTED_EDGE ( 'NONE', *, *, #12377, .F. ) ;
#10563 = CARTESIAN_POINT ( 'NONE',  ( 70.00000000000000000, -87.33333333333334281, 153.0000000000000000 ) ) ;
#10564 = DIRECTION ( 'NONE',  ( 1.000000000000000000, 0.000000000000000000, 0.000000000000000000 ) ) ;
#10565 = CARTESIAN_POINT ( 'NONE',  ( 110.0000000000000000, -74.99999999999998579, 0.000000000000000000 ) ) ;
#10566 = CARTESIAN_POINT ( 'NONE',  ( 0.2500000000000002220, 0.000000000000000000, 4.000000000000021316 ) ) ;
#10567 = CARTESIAN_POINT ( 'NONE',  ( 90.00000000000000000, 95.00000000000000000, 0.000000000000000000 ) ) ;
#10568 = EDGE_CURVE ( 'NONE', #19646, #6763, #1731, .T. ) ;
#10569 = EDGE_LOOP ( 'NONE', ( #18360, #12582, #1898, #23552 ) ) ;
#10570 = EDGE_CURVE ( 'NONE', #20887, #13282, #14285, .T. ) ;
#10571 = CIRCLE ( 'NONE', #132, 2.041999999999999815 ) ;
#10572 = CARTESIAN_POINT ( 'NONE',  ( 7.500000000000000000, -2.571118828324946648, -0.3627527587569098766 ) ) ;
#10573 = EDGE_CURVE ( 'NONE', #321, #12103, #23502, .T. ) ;
#10574 = VERTEX_POINT ( 'NONE', #1978 ) ;
#10575 = CARTESIAN_POINT ( 'NONE',  ( 0.000000000000000000, 0.000000000000000000, 0.000000000000000000 ) ) ;
#10576 = DIRECTION ( 'NONE',  ( 1.000000000000000000, 0.000000000000000000, 0.000000000000000000 ) ) ;
#10577 = CONTEXT_DEPENDENT_SHAPE_REPRESENTATION ( #14830, #2907 ) ;
#10578 = ORIENTED_EDGE ( 'NONE', *, *, #5363, .T. ) ;
#10579 = LINE ( 'NONE', #7238, #7121 ) ;
#10580 = ORIENTED_EDGE ( 'NONE', *, *, #6239, .T. ) ;
#10581 = CARTESIAN_POINT ( 'NONE',  ( -128.2758413234845705, 87.00805048166530753, -32.43450926607476958 ) ) ;
#10582 = DIRECTION ( 'NONE',  ( -5.478074134663601247E-16, 1.000000000000000000, 0.000000000000000000 ) ) ;
#10583 = ORIENTED_EDGE ( 'NONE', *, *, #18003, .T. ) ;
#10584 = DIRECTION ( 'NONE',  ( -1.000000000000000000, 0.000000000000000000, 0.000000000000000000 ) ) ;
#10585 = LINE ( 'NONE', #13987, #3421 ) ;
#10586 = CARTESIAN_POINT ( 'NONE',  ( -7.897850199329715437, 1.533397866934075759, -7.634054012537968781 ) ) ;
#10587 = AXIS2_PLACEMENT_3D ( 'NONE', #19784, #18106, #16183 ) ;
#10588 = PRODUCT_DEFINITION_SHAPE ( 'NONE', 'NONE',  #23812 ) ;
#10589 = AXIS2_PLACEMENT_3D ( 'NONE', #2294, #4919, #10376 ) ;
#10590 = FACE_OUTER_BOUND ( 'NONE', #1069, .T. ) ;
#10591 = CARTESIAN_POINT ( 'NONE',  ( 29.55500000000002458, 0.000000000000000000, -6.938893903907228378E-15 ) ) ;
#10592 = DIRECTION ( 'NONE',  ( -1.000000000000000000, -0.000000000000000000, -0.000000000000000000 ) ) ;
#10593 = DIRECTION ( 'NONE',  ( 0.000000000000000000, -1.177509268541832635E-16, 1.000000000000000000 ) ) ;
#10594 = VERTEX_POINT ( 'NONE', #9364 ) ;
#10595 = DIRECTION ( 'NONE',  ( -0.000000000000000000, -0.000000000000000000, 1.000000000000000000 ) ) ;
#10596 = CARTESIAN_POINT ( 'NONE',  ( 0.1404048886732821022, 4.699864953788070565, -3.686887068327037387 ) ) ;
#10597 = ORIENTED_EDGE ( 'NONE', *, *, #21478, .F. ) ;
#10598 = ORIENTED_EDGE ( 'NONE', *, *, #10682, .F. ) ;
#10599 = DIRECTION ( 'NONE',  ( -1.000000000000000000, -0.000000000000000000, -0.000000000000000000 ) ) ;
#10600 = DIRECTION ( 'NONE',  ( 0.000000000000000000, -2.618450529776326854E-15, -1.000000000000000000 ) ) ;
#10601 = CARTESIAN_POINT ( 'NONE',  ( 93.00000000000000000, -149.9999999999996874, 129.9038105676659711 ) ) ;
#10602 = EDGE_CURVE ( 'NONE', #21414, #9294, #16722, .T. ) ;
#10603 = VECTOR ( 'NONE', #2616, 1000.000000000000000 ) ;
#10604 = AXIS2_PLACEMENT_3D ( 'NONE', #18859, #13248, #18731 ) ;
#10605 = DIRECTION ( 'NONE',  ( -0.000000000000000000, -0.000000000000000000, -1.000000000000000000 ) ) ;
#10606 = CARTESIAN_POINT ( 'NONE',  ( -284.6730547946947354, 270.1059783239178387, -146.0571358042175802 ) ) ;
#10607 = ORIENTED_EDGE ( 'NONE', *, *, #9669, .T. ) ;
#10608 = DIRECTION ( 'NONE',  ( 1.350636282998972974E-14, 0.000000000000000000, -1.000000000000000000 ) ) ;
#10609 = ORIENTED_EDGE ( 'NONE', *, *, #21588, .T. ) ;
#10610 = CARTESIAN_POINT ( 'NONE',  ( 50.00000000000000000, 0.000000000000000000, 0.000000000000000000 ) ) ;
#10611 = LINE ( 'NONE', #6838, #15781 ) ;
#10612 = SURFACE_SIDE_STYLE ('',( #1527 ) ) ;
#10613 = ORIENTED_EDGE ( 'NONE', *, *, #2996, .T. ) ;
#10614 = LINE ( 'NONE', #17954, #9661 ) ;
#10615 = B_SPLINE_CURVE_WITH_KNOTS ( 'NONE', 3,
 ( #11928, #9849, #22753, #13260, #9971, #6087, #6218, #17445, #11685, #17207, #20825, #5852, #5968, #13377, #17084, #13624, #15530, #4020, #21057, #7903, #19238, #9730, #7656, #7785, #20567, #11434, #13508, #2212, #4282, #18994, #2457, #9604 ),
 .UNSPECIFIED., .F., .F.,
 ( 4, 2, 2, 2, 2, 2, 2, 2, 2, 2, 2, 2, 2, 2, 2, 4 ),
 ( 1.430489624538199204E-17, 0.0004914281572963898059, 0.0009828563145927653004, 0.001474284471889140795, 0.001965712629185516289, 0.002457140786481891784, 0.002948568943778267278, 0.003931425258371017833, 0.004422853415667393762, 0.004914281572963768822, 0.005405709730260143883, 0.005897137887556519811, 0.006388566044852895739, 0.006879994202149270800, 0.007371422359445645861, 0.007862850516742021789 ),
 .UNSPECIFIED. ) ;
#10616 = CARTESIAN_POINT ( 'NONE',  ( 34.99999999999999289, 0.000000000000000000, 0.000000000000000000 ) ) ;
#10617 = DIRECTION ( 'NONE',  ( 0.000000000000000000, 0.4999999999999991118, -0.8660254037844391517 ) ) ;
#10618 = DIRECTION ( 'NONE',  ( 0.000000000000000000, 2.618450529776326854E-15, 1.000000000000000000 ) ) ;
#10619 = AXIS2_PLACEMENT_3D ( 'NONE', #17668, #15754, #1128 ) ;
#10620 = DIRECTION ( 'NONE',  ( 0.000000000000000000, 0.4999999999999992784, -0.8660254037844390407 ) ) ;
#10621 = CARTESIAN_POINT ( 'NONE',  ( 0.000000000000000000, 0.000000000000000000, 90.00000000000000000 ) ) ;
#10622 = DIRECTION ( 'NONE',  ( 1.000000000000000000, -0.000000000000000000, -0.000000000000000000 ) ) ;
#10623 = EDGE_LOOP ( 'NONE', ( #11410, #20898 ) ) ;
#10624 = VECTOR ( 'NONE', #12966, 1000.000000000000000 ) ;
#10625 = VERTEX_POINT ( 'NONE', #14921 ) ;
#10626 = DIRECTION ( 'NONE',  ( 0.000000000000000000, -1.000000000000000000, 0.000000000000000000 ) ) ;
#10627 = DIRECTION ( 'NONE',  ( 1.000000000000000000, -0.000000000000000000, -0.000000000000000000 ) ) ;
#10628 = ORIENTED_EDGE ( 'NONE', *, *, #22635, .F. ) ;
#10629 = CIRCLE ( 'NONE', #19850, 2.041999999999999815 ) ;
#10630 = DIRECTION ( 'NONE',  ( -0.000000000000000000, -0.000000000000000000, 1.000000000000000000 ) ) ;
#10631 = FACE_BOUND ( 'NONE', #17485, .T. ) ;
#10632 = ORIENTED_EDGE ( 'NONE', *, *, #8978, .F. ) ;
#10633 = CARTESIAN_POINT ( 'NONE',  ( -69.99999999999997158, -87.33333333333338544, 3.000000000000000000 ) ) ;
#10634 = EDGE_CURVE ( 'NONE', #15403, #16905, #18059, .T. ) ;
#10635 = CARTESIAN_POINT ( 'NONE',  ( -1.499999046620369203, 9.887721681869660273, 200.0000060000000133 ) ) ;
#10636 = EDGE_LOOP ( 'NONE', ( #9331, #11990 ) ) ;
#10637 = DIRECTION ( 'NONE',  ( 0.000000000000000000, 0.000000000000000000, 1.000000000000000000 ) ) ;
#10638 = ADVANCED_FACE ( 'NONE', ( #16261 ), #7062, .T. ) ;
#10639 = APPLICATION_CONTEXT ( 'automotive_design' ) ;
#10640 = VECTOR ( 'NONE', #21475, 1000.000000000000000 ) ;
#10641 = ORIENTED_EDGE ( 'NONE', *, *, #13451, .F. ) ;
#10642 = DIRECTION ( 'NONE',  ( -0.000000000000000000, 1.000000000000000000, -0.000000000000000000 ) ) ;
#10643 = ADVANCED_FACE ( 'NONE', ( #4277 ), #13144, .T. ) ;
#10644 = ADVANCED_FACE ( 'NONE', ( #20818 ), #18268, .F. ) ;
#10645 = DIRECTION ( 'NONE',  ( 0.8090169943749468962, 0.5877852522924740253, 0.000000000000000000 ) ) ;
#10646 = ORIENTED_EDGE ( 'NONE', *, *, #1075, .F. ) ;
#10647 = EDGE_LOOP ( 'NONE', ( #17312, #14255, #17799, #16736 ) ) ;
#10648 = CARTESIAN_POINT ( 'NONE',  ( 133.4872637682709069, 78.77924338078965150, -27.82770220384453097 ) ) ;
#10649 = CIRCLE ( 'NONE', #17551, 2.500000000000002220 ) ;
#10650 = CARTESIAN_POINT ( 'NONE',  ( -39.99999999999999289, 100.0000000000000000, 114.9999999999999574 ) ) ;
#10651 = DIRECTION ( 'NONE',  ( 1.000000000000000000, 0.000000000000000000, 0.000000000000000000 ) ) ;
#10652 = DIRECTION ( 'NONE',  ( 0.000000000000000000, -1.000000000000000000, 0.000000000000000000 ) ) ;
#10653 = FACE_BOUND ( 'NONE', #1353, .T. ) ;
#10654 = B_SPLINE_CURVE_WITH_KNOTS ( 'NONE', 3,
 ( #7586, #22075, #9309, #16660, #20148, #3494, #9061, #11015, #5542, #18335, #22189, #1788, #115, #14979, #5662, #10773, #16537, #16421, #13073, #1572, #5306, #21840, #20504, #12720, #20039, #6, #13569, #356, #6144, #4203, #20879, #18800, #4333, #19167 ),
 .UNSPECIFIED., .F., .F.,
 ( 4, 2, 2, 2, 2, 2, 2, 2, 2, 2, 2, 2, 2, 2, 2, 2, 4 ),
 ( 0.5000000000000000000, 0.5312500000000000000, 0.5625000000000000000, 0.5937500000000000000, 0.6250000000000000000, 0.6562500000000000000, 0.6875000000000000000, 0.7187500000000000000, 0.7500000000000000000, 0.7812500000000000000, 0.8125000000000000000, 0.8437500000000000000, 0.8750000000000000000, 0.9062500000000000000, 0.9375000000000000000, 0.9687500000000000000, 1.000000000000000000 ),
 .UNSPECIFIED. ) ;
#10655 = EDGE_CURVE ( 'NONE', #8474, #21138, #2336, .T. ) ;
#10656 = ORIENTED_EDGE ( 'NONE', *, *, #14684, .T. ) ;
#10657 = FACE_BOUND ( 'NONE', #23043, .T. ) ;
#10658 = VECTOR ( 'NONE', #11351, 1000.000000000000000 ) ;
#10659 = ORIENTED_EDGE ( 'NONE', *, *, #2643, .T. ) ;
#10660 = PLANE ( 'NONE',  #12554 ) ;
#10661 = CIRCLE ( 'NONE', #1319, 2.649999999999999467 ) ;
#10662 = CARTESIAN_POINT ( 'NONE',  ( 21.00000000000000355, 2.516649172247811061E-16, -2.055000000000000160 ) ) ;
#10663 = VERTEX_POINT ( 'NONE', #18743 ) ;
#10664 = PLANE ( 'NONE',  #4058 ) ;
#10665 = ORIENTED_EDGE ( 'NONE', *, *, #5807, .F. ) ;
#10666 = AXIS2_PLACEMENT_3D ( 'NONE', #13157, #15174, #11566 ) ;
#10667 = DIRECTION ( 'NONE',  ( 0.000000000000000000, 0.000000000000000000, 1.000000000000000000 ) ) ;
#10668 = ADVANCED_FACE ( 'NONE', ( #8020 ), #7898, .F. ) ;
#10669 = EDGE_LOOP ( 'NONE', ( #19915, #22319, #6548, #13891 ) ) ;
#10670 = EDGE_CURVE ( 'NONE', #21826, #8393, #11194, .T. ) ;
#10671 = DIRECTION ( 'NONE',  ( 0.000000000000000000, 0.000000000000000000, -1.000000000000000000 ) ) ;
#10672 = EDGE_CURVE ( 'NONE', #18124, #160, #21960, .T. ) ;
#10673 = CARTESIAN_POINT ( 'NONE',  ( -280.6225751257470620, 269.5484459290826180, 146.3429506979392443 ) ) ;
#10674 = CARTESIAN_POINT ( 'NONE',  ( -155.0000000000000284, -204.4690652294806057, 30.00000000000648015 ) ) ;
#10675 = AXIS2_PLACEMENT_3D ( 'NONE', #7768, #22481, #5944 ) ;
#10676 = DIRECTION ( 'NONE',  ( 3.202566417187928841E-16, -1.000000000000000000, 3.469446951953614583E-15 ) ) ;
#10677 = ADVANCED_FACE ( 'NONE', ( #21174 ), #8616, .F. ) ;
#10678 = PRODUCT_RELATED_PRODUCT_CATEGORY ( 'part', '', ( #12733 ) ) ;
#10679 = DIRECTION ( 'NONE',  ( -0.000000000000000000, -0.000000000000000000, 1.000000000000000000 ) ) ;
#10680 = ORIENTED_EDGE ( 'NONE', *, *, #9898, .F. ) ;
#10681 = CARTESIAN_POINT ( 'NONE',  ( 153.5653415408401941, -1122.352966361446079, -29.99999999999322498 ) ) ;
#10682 = EDGE_CURVE ( 'NONE', #21824, #12819, #15988, .T. ) ;
#10683 = PRODUCT_DEFINITION_SHAPE ( 'NONE', 'NONE',  #23828 ) ;
#10685 = VERTEX_POINT ( 'NONE', #10199 ) ;
#10684 = ORIENTED_EDGE ( 'NONE', *, *, #1762, .F. ) ;
#10686 = DIRECTION ( 'NONE',  ( 1.000000000000000000, 2.832769448823979947E-16, -2.832769448823989808E-16 ) ) ;
#10687 = CARTESIAN_POINT ( 'NONE',  ( 145.9999999999998010, -209.9999999999996874, 30.00000000000641620 ) ) ;
#10688 = AXIS2_PLACEMENT_3D ( 'NONE', #12797, #7063, #14451 ) ;
#10689 = DIRECTION ( 'NONE',  ( 0.000000000000000000, -1.000000000000000000, 0.000000000000000000 ) ) ;
#10690 = DIRECTION ( 'NONE',  ( -0.000000000000000000, 1.000000000000000000, -3.469446951953613794E-15 ) ) ;
#10691 = DIRECTION ( 'NONE',  ( 0.000000000000000000, -0.5000000000000009992, -0.8660254037844380415 ) ) ;
#10692 = ORIENTED_EDGE ( 'NONE', *, *, #12548, .F. ) ;
#10693 = CARTESIAN_POINT ( 'NONE',  ( -287.4000000000014552, -127.0000000000000568, -146.4928932188134070 ) ) ;
#10694 = ORIENTED_EDGE ( 'NONE', *, *, #2838, .F. ) ;
#10695 = CARTESIAN_POINT ( 'NONE',  ( -56.99999999999995026, -65.27838379715711881, 65.27838379715736039 ) ) ;
#10696 = FACE_BOUND ( 'NONE', #1061, .T. ) ;
#10697 = ORIENTED_EDGE ( 'NONE', *, *, #279, .F. ) ;
#10698 =( BOUNDED_SURFACE ( )  B_SPLINE_SURFACE ( 3, 2, ( 
 ( #18203, #95, #7445 ),
 ( #20005, #18422, #12927 ),
 ( #9036, #3688, #19890 ),
 ( #7200, #20239, #16395 ),
 ( #22166, #16748, #23746 ),
 ( #14589, #5640, #13048 ),
 ( #16508, #3342, #1881 ),
 ( #20350, #3813, #11102 ) ),
 .UNSPECIFIED., .F., .F., .F. ) 
 B_SPLINE_SURFACE_WITH_KNOTS ( ( 4, 2, 2, 4 ),
 ( 3, 3 ),
 ( 0.03861844051980971304, 0.04325213341840643266, 0.04556897986770479247, 0.04788582631700314535 ),
 ( 0.000000000000000000, 1.000000000000000000 ),
 .UNSPECIFIED. ) 
 GEOMETRIC_REPRESENTATION_ITEM ( )  RATIONAL_B_SPLINE_SURFACE ( (
 ( 1.000000000000000000, 0.8047781759831919013, 1.000000000000000000),
 ( 1.000000000000000000, 0.8123762462802479600, 1.000000000000000000),
 ( 1.000000000000000000, 0.8190659850620179983, 1.000000000000000000),
 ( 1.000000000000000000, 0.8191937571011910224, 1.000000000000000000),
 ( 1.000000000000000000, 0.8176092952781196521, 1.000000000000000000),
 ( 1.000000000000000000, 0.8122962088595743202, 1.000000000000000000),
 ( 1.000000000000000000, 0.8086311330828506172, 1.000000000000000000),
 ( 1.000000000000000000, 0.8047712282214323221, 1.000000000000000000) ) ) 
 REPRESENTATION_ITEM ( '' )  SURFACE ( )  );
#10699 = ORIENTED_EDGE ( 'NONE', *, *, #5493, .F. ) ;
#10700 = CARTESIAN_POINT ( 'NONE',  ( -7.640563834021360018E-16, -9.147862274876560562, -8.047472243342937759 ) ) ;
#10701 = CARTESIAN_POINT ( 'NONE',  ( -282.2000000000000455, 267.7999999999999545, 146.4928932188134354 ) ) ;
#10702 = VERTEX_POINT ( 'NONE', #15524 ) ;
#10703 = DIRECTION ( 'NONE',  ( -1.000000000000000000, -0.000000000000000000, -0.000000000000000000 ) ) ;
#10704 = CARTESIAN_POINT ( 'NONE',  ( 0.000000000000000000, 0.000000000000000000, 100.0000000000000000 ) ) ;
#10705 = DIRECTION ( 'NONE',  ( -0.5000000000000016653, 0.8660254037844378194, 0.000000000000000000 ) ) ;
#10706 = LINE ( 'NONE', #1493, #12551 ) ;
#10707 = ADVANCED_FACE ( 'NONE', ( #12054 ), #21403, .F. ) ;
#10708 = EDGE_CURVE ( 'NONE', #17386, #8380, #8258, .T. ) ;
#10709 = CARTESIAN_POINT ( 'NONE',  ( 112.7436279071518754, 91.18044947429078206, -2.775557561562891351E-14 ) ) ;
#10710 = EDGE_CURVE ( 'NONE', #21875, #306, #23214, .T. ) ;
#10711 = LINE ( 'NONE', #21670, #1884 ) ;
#10712 = VERTEX_POINT ( 'NONE', #8371 ) ;
#10713 =( NAMED_UNIT ( * ) PLANE_ANGLE_UNIT ( ) SI_UNIT ( $, .RADIAN. ) );
#10714 = FACE_OUTER_BOUND ( 'NONE', #2166, .T. ) ;
#10715 = CARTESIAN_POINT ( 'NONE',  ( 6.250000000000000000, -5.051814855409237026, -7.198902722707430257 ) ) ;
#10716 = CIRCLE ( 'NONE', #2573, 0.3000000000000051514 ) ;
#10717 = ORIENTED_EDGE ( 'NONE', *, *, #14410, .T. ) ;
#10718 = CARTESIAN_POINT ( 'NONE',  ( -31.74999999999995737, 3.061616997868383634E-16, -2.500000000000000444 ) ) ;
#10719 = CARTESIAN_POINT ( 'NONE',  ( 0.000000000000000000, 0.000000000000000000, 0.000000000000000000 ) ) ;
#10720 = AXIS2_PLACEMENT_3D ( 'NONE', #23638, #8806, #14142 ) ;
#10721 = CARTESIAN_POINT ( 'NONE',  ( -282.6188186979287025, 272.3436892194421262, 145.4976310729378213 ) ) ;
#10722 = CARTESIAN_POINT ( 'NONE',  ( 132.8404720734533555, 79.86494211668886578, -32.49999999999351985 ) ) ;
#10723 = CARTESIAN_POINT ( 'NONE',  ( -288.2000000000013529, -89.99999999999897682, 24.33333333333333215 ) ) ;
#10724 = ORIENTED_EDGE ( 'NONE', *, *, #4594, .T. ) ;
#10725 = DIRECTION ( 'NONE',  ( -1.000000000000000000, 0.000000000000000000, 0.000000000000000000 ) ) ;
#10726 = ORIENTED_EDGE ( 'NONE', *, *, #15767, .F. ) ;
#10727 = CARTESIAN_POINT ( 'NONE',  ( 1.999999999999998224, -3.464101615137772594, -3.142992957459239012 ) ) ;
#10728 = DIRECTION ( 'NONE',  ( -1.000000000000000000, 0.000000000000000000, 0.000000000000000000 ) ) ;
#10729 = SURFACE_STYLE_USAGE ( .BOTH. , #10612 ) ;
#10730 = EDGE_LOOP ( 'NONE', ( #8672, #7149, #4717, #9376 ) ) ;
#10731 = CIRCLE ( 'NONE', #14558, 4.000000000000000000 ) ;
#10732 = CARTESIAN_POINT ( 'NONE',  ( -7.894787914004607998, -1.230850257101226302E-13, -7.591390474663425536 ) ) ;
#10733 = DIRECTION ( 'NONE',  ( 0.000000000000000000, 0.000000000000000000, -1.000000000000000000 ) ) ;
#10734 = LINE ( 'NONE', #23732, #11192 ) ;
#10735 = CARTESIAN_POINT ( 'NONE',  ( -122.8605704798721945, 82.74225173005939382, -29.99999999999356604 ) ) ;
#10737 = CIRCLE ( 'NONE', #1062, 4.250000000000000000 ) ;
#10736 = DIRECTION ( 'NONE',  ( 0.000000000000000000, -1.000000000000000000, 0.000000000000000000 ) ) ;
#10738 = CARTESIAN_POINT ( 'NONE',  ( 50.00000000000000000, 0.000000000000000000, 0.000000000000000000 ) ) ;
#10739 = AXIS2_PLACEMENT_3D ( 'NONE', #18104, #12589, #21827 ) ;
#10740 = CARTESIAN_POINT ( 'NONE',  ( 93.00000000000000000, -74.99999999999998579, 129.9038105676659711 ) ) ;
#10741 = AXIS2_PLACEMENT_3D ( 'NONE', #18549, #21933, #1655 ) ;
#10742 = VERTEX_POINT ( 'NONE', #13846 ) ;
#10743 = ORIENTED_EDGE ( 'NONE', *, *, #1633, .F. ) ;
#10744 = FACE_OUTER_BOUND ( 'NONE', #18924, .T. ) ;
#10745 = CARTESIAN_POINT ( 'NONE',  ( 72.64999999999999147, -112.6666666666666714, 3.000000000000001332 ) ) ;
#10746 = EDGE_LOOP ( 'NONE', ( #9335, #3901, #9347, #19071 ) ) ;
#10747 = DIRECTION ( 'NONE',  ( 0.000000000000000000, 0.000000000000000000, -1.000000000000000000 ) ) ;
#10748 = LINE ( 'NONE', #5414, #296 ) ;
#10749 = CIRCLE ( 'NONE', #6078, 2.649999999999985700 ) ;
#10750 = ORIENTED_EDGE ( 'NONE', *, *, #1574, .T. ) ;
#10751 = CARTESIAN_POINT ( 'NONE',  ( 5.200000000000020606, 0.000000000000000000, -6.938893903907228378E-15 ) ) ;
#10752 = DIRECTION ( 'NONE',  ( -0.000000000000000000, -0.000000000000000000, 1.000000000000000000 ) ) ;
#10753 = ORIENTED_EDGE ( 'NONE', *, *, #18930, .F. ) ;
#10754 = AXIS2_PLACEMENT_3D ( 'NONE', #4498, #12040, #865 ) ;
#10755 = DIRECTION ( 'NONE',  ( -2.775557561562891351E-17, 1.000000000000000000, 4.694093751100962712E-16 ) ) ;
#10756 = AXIS2_PLACEMENT_3D ( 'NONE', #16035, #8552, #23512 ) ;
#10757 = CIRCLE ( 'NONE', #7249, 2.499999999999998668 ) ;
#10758 = ORIENTED_EDGE ( 'NONE', *, *, #23154, .T. ) ;
#10759 = DIRECTION ( 'NONE',  ( 1.000000000000000000, 0.000000000000000000, 0.000000000000000000 ) ) ;
#10760 = DIRECTION ( 'NONE',  ( 0.8090169943749468962, 0.5877852522924740253, 0.000000000000000000 ) ) ;
#10761 = ORIENTED_EDGE ( 'NONE', *, *, #14434, .T. ) ;
#10762 = ORIENTED_EDGE ( 'NONE', *, *, #12244, .F. ) ;
#10763 = EDGE_CURVE ( 'NONE', #17922, #6350, #13138, .T. ) ;
#10764 = CARTESIAN_POINT ( 'NONE',  ( 280.6847249064868492, 273.0299999999999159, -145.1244295015775378 ) ) ;
#10765 = DIRECTION ( 'NONE',  ( 1.221966984364620947E-29, 3.495664435217746987E-15, -1.000000000000000000 ) ) ;
#10766 = DIRECTION ( 'NONE',  ( 0.000000000000000000, 0.000000000000000000, 1.000000000000000000 ) ) ;
#10767 = FACE_OUTER_BOUND ( 'NONE', #14271, .T. ) ;
#10768 = DIRECTION ( 'NONE',  ( -0.000000000000000000, -0.000000000000000000, 1.000000000000000000 ) ) ;
#10769 = EDGE_CURVE ( 'NONE', #21577, #2989, #11918, .T. ) ;
#10770=STYLED_ITEM('',(#23913),#19817);
#10771 = VERTEX_POINT ( 'NONE', #17541 ) ;
#10772 = AXIS2_PLACEMENT_3D ( 'NONE', #14578, #22045, #20226 ) ;
#10773 = CARTESIAN_POINT ( 'NONE',  ( -3.272451888078292903, -24.83884780301427497, 145.0000120000000265 ) ) ;
#10774 = PRESENTATION_STYLE_ASSIGNMENT (( #3495 ) ) ;
#10775 = EDGE_CURVE ( 'NONE', #21417, #16062, #17659, .T. ) ;
#10776 = AXIS2_PLACEMENT_3D ( 'NONE', #15715, #13937, #8462 ) ;
#10777 = CIRCLE ( 'NONE', #16539, 145.0000000000000284 ) ;
#10778 = ADVANCED_FACE ( 'NONE', ( #10456 ), #15633, .T. ) ;
#10779 = CIRCLE ( 'NONE', #341, 2.649999999999975486 ) ;
#10780 = CARTESIAN_POINT ( 'NONE',  ( -31.74999999999995737, 0.000000000000000000, 8.000000000000000000 ) ) ;
#10781 = FACE_OUTER_BOUND ( 'NONE', #23305, .T. ) ;
#10782 = EDGE_LOOP ( 'NONE', ( #2830, #3469, #3754, #16703 ) ) ;
#10783 = CARTESIAN_POINT ( 'NONE',  ( 158.0000000000000284, -500.0000000000000000, -27.34999999999998721 ) ) ;
#10784 = EDGE_LOOP ( 'NONE', ( #14748, #17992, #591, #6964 ) ) ;
#10785 = B_SPLINE_SURFACE_WITH_KNOTS ( 'NONE', 1, 3, ( 
 ( #14320, #4106, #15250, #2308, #2175, #13463, #9564, #5694, #5932, #11519 ),
 ( #22354, #16578, #15136, #16927, #22466, #7758, #396, #9448, #3748, #13228 ),
 ( #16692, #11164, #5574, #9213, #18493, #20776, #4240, #9699, #13340, #22584 ),
 ( #12985, #6047, #17053, #18365, #14770, #22103, #44, #7500, #1820, #7389 ) ),
 .UNSPECIFIED., .F., .F., .F.,
 ( 2, 1, 1, 2 ),
 ( 4, 2, 2, 2, 4 ),
 ( -0.01000000000000000021, 0.000000000000000000, 1.000000000000000000, 1.010099999999999998 ),
 ( 0.000000000000000000, 0.2500000000000000000, 0.5000000000000000000, 0.7500000000000000000, 1.000000000000000000 ),
 .UNSPECIFIED. ) ;
#10786 = MECHANICAL_DESIGN_GEOMETRIC_PRESENTATION_REPRESENTATION (  '', ( #735 ), #22710 ) ;
#10788 = VECTOR ( 'NONE', #23597, 1000.000000000000000 ) ;
#10787 = STYLED_ITEM ( 'NONE', ( #10774 ), #22256 ) ;
#10789 = FACE_OUTER_BOUND ( 'NONE', #21465, .T. ) ;
#10790 = AXIS2_PLACEMENT_3D ( 'NONE', #10254, #22797, #13562 ) ;
#10791 = ORIENTED_EDGE ( 'NONE', *, *, #11069, .F. ) ;
#10792=STYLED_ITEM('',(#23927),#4076);
#10793 = DIRECTION ( 'NONE',  ( 1.000000000000000000, -0.000000000000000000, -0.000000000000000000 ) ) ;
#10794 = CARTESIAN_POINT ( 'NONE',  ( 7.500000000000007105, -4.330127018922196314, -7.564338275809341816 ) ) ;
#10795 = AXIS2_PLACEMENT_3D ( 'NONE', #17796, #10690, #1239 ) ;
#10796 = CARTESIAN_POINT ( 'NONE',  ( -288.2000000000013529, -89.99999999999896261, -40.33333333333332860 ) ) ;
#10797 = CARTESIAN_POINT ( 'NONE',  ( 125.5946212300928266, -1090.835042168281461, -28.33934113061012283 ) ) ;
#10798 = PLANE ( 'NONE',  #21153 ) ;
#10799 = VERTEX_POINT ( 'NONE', #15878 ) ;
#10800 = CARTESIAN_POINT ( 'NONE',  ( -288.2000000000006708, 90.00000000000100897, 34.99999999999999289 ) ) ;
#10802 = ORIENTED_EDGE ( 'NONE', *, *, #8245, .T. ) ;
#10801 = VERTEX_POINT ( 'NONE', #23095 ) ;
#10803 = VECTOR ( 'NONE', #9585, 1000.000000000000000 ) ;
#10805 = VECTOR ( 'NONE', #20662, 1000.000000000000000 ) ;
#10804 = DIRECTION ( 'NONE',  ( -1.000000000000000000, 0.000000000000000000, 0.000000000000000000 ) ) ;
#10807 = AXIS2_PLACEMENT_3D ( 'NONE', #1838, #18383, #12889 ) ;
#10806 =( GEOMETRIC_REPRESENTATION_CONTEXT ( 3 ) GLOBAL_UNCERTAINTY_ASSIGNED_CONTEXT ( ( #5544 ) ) GLOBAL_UNIT_ASSIGNED_CONTEXT ( ( #10344, #10713, #16257 ) ) REPRESENTATION_CONTEXT ( 'NONE', 'WORKASPACE' ) );
#10808 = DIRECTION ( 'NONE',  ( 0.000000000000000000, -0.000000000000000000, 1.000000000000000000 ) ) ;
#10809 = CYLINDRICAL_SURFACE ( 'NONE', #14224, 2.649999999999971934 ) ;
#10810 = CONICAL_SURFACE ( 'NONE', #15037, 2.059999999999998721, 0.9599310885968738161 ) ;
#10811 = ADVANCED_FACE ( 'NONE', ( #13974 ), #3065, .F. ) ;
#10812 = AXIS2_PLACEMENT_3D ( 'NONE', #6705, #21426, #17815 ) ;
#10813 = VECTOR ( 'NONE', #13731, 1000.000000000000000 ) ;
#10814 = AXIS2_PLACEMENT_3D ( 'NONE', #8409, #15792, #23137 ) ;
#10815 = AXIS2_PLACEMENT_3D ( 'NONE', #12449, #1276, #16268 ) ;
#10816 = VERTEX_POINT ( 'NONE', #10095 ) ;
#10817 = EDGE_CURVE ( 'NONE', #6073, #12669, #17436, .T. ) ;
#10818 = DIRECTION ( 'NONE',  ( -0.000000000000000000, -0.000000000000000000, 1.000000000000000000 ) ) ;
#10819 = DIRECTION ( 'NONE',  ( 1.000000000000000000, 0.000000000000000000, 0.000000000000000000 ) ) ;
#10820 = ADVANCED_FACE ( 'NONE', ( #12158 ), #9241, .T. ) ;
#10821 = ORIENTED_EDGE ( 'NONE', *, *, #5335, .T. ) ;
#10822 = LINE ( 'NONE', #5114, #13115 ) ;
#10823 = CARTESIAN_POINT ( 'NONE',  ( 1.411581201560190495E-15, 4.862606272033091592, -3.745885042887436622 ) ) ;
#10824 = EDGE_CURVE ( 'NONE', #12957, #18256, #8091, .T. ) ;
#10825 = CONTEXT_DEPENDENT_SHAPE_REPRESENTATION ( #12849, #4861 ) ;
#10826 = ORIENTED_EDGE ( 'NONE', *, *, #7996, .T. ) ;
#10827 = ORIENTED_EDGE ( 'NONE', *, *, #7628, .F. ) ;
#10828 = CARTESIAN_POINT ( 'NONE',  ( 125.9649699199276967, -1090.320686186013290, 30.16873261443294041 ) ) ;
#10830 = VECTOR ( 'NONE', #20893, 1000.000000000000000 ) ;
#10829 = AXIS2_PLACEMENT_3D ( 'NONE', #17195, #15394, #22846 ) ;
#10831 = VERTEX_POINT ( 'NONE', #4094 ) ;
#10832 = CARTESIAN_POINT ( 'NONE',  ( -146.0000000000005400, -784.4690652294799520, -32.05499999999356930 ) ) ;
#10833 = MECHANICAL_DESIGN_GEOMETRIC_PRESENTATION_REPRESENTATION (  '', ( #1542 ), #18126 ) ;
#10834 = AXIS2_PLACEMENT_3D ( 'NONE', #16691, #9809, #7618 ) ;
#10835 = DIRECTION ( 'NONE',  ( -1.000000000000000000, 0.000000000000000000, 0.000000000000000000 ) ) ;
#10836 = AXIS2_PLACEMENT_3D ( 'NONE', #13584, #22816, #13217 ) ;
#10837 = VECTOR ( 'NONE', #6709, 1000.000000000000000 ) ;
#10838 = CARTESIAN_POINT ( 'NONE',  ( 1.500000000000000000, 12.00000000000000000, -50.00000000000000000 ) ) ;
#10839 = DIRECTION ( 'NONE',  ( -1.000000000000000000, 0.000000000000000000, 0.000000000000000000 ) ) ;
#10840 = CYLINDRICAL_SURFACE ( 'NONE', #11984, 2.199999999999979750 ) ;
#10841 = AXIS2_PLACEMENT_3D ( 'NONE', #10566, #17658, #1122 ) ;
#10842 = ORIENTED_EDGE ( 'NONE', *, *, #8034, .F. ) ;
#10843 =( LENGTH_UNIT ( ) NAMED_UNIT ( * ) SI_UNIT ( .MILLI., .METRE. ) );
#10844 = EDGE_CURVE ( 'NONE', #18342, #8126, #724, .T. ) ;
#10845 = LINE ( 'NONE', #14556, #1452 ) ;
#10846 = CYLINDRICAL_SURFACE ( 'NONE', #12023, 21.02499999999999503 ) ;
#10847 = EDGE_LOOP ( 'NONE', ( #11897, #14795, #1416, #16051 ) ) ;
#10848 = PLANE ( 'NONE',  #19251 ) ;
#10849 = CARTESIAN_POINT ( 'NONE',  ( 155.0000000000000284, -500.0000000000000000, 32.50000000000001421 ) ) ;
#10850 = AXIS2_PLACEMENT_3D ( 'NONE', #19909, #23650, #19675 ) ;
#10851 = VECTOR ( 'NONE', #23745, 1000.000000000000000 ) ;
#10852 = AXIS2_PLACEMENT_3D ( 'NONE', #23290, #17503, #15711 ) ;
#10853 = DIRECTION ( 'NONE',  ( -1.000000000000000000, -2.775557561562891351E-17, 0.000000000000000000 ) ) ;
#10854 = AXIS2_PLACEMENT_3D ( 'NONE', #22740, #15876, #877 ) ;
#10855 = ADVANCED_FACE ( 'NONE', ( #2656 ), #18823, .T. ) ;
#10856 = CARTESIAN_POINT ( 'NONE',  ( -34.75000000000005684, 100.0000000000000000, 145.0000000000000000 ) ) ;
#10857 = EDGE_CURVE ( 'NONE', #16244, #17193, #20033, .T. ) ;
#10858 = CARTESIAN_POINT ( 'NONE',  ( 280.9020829022173302, 270.8299054689547347, -149.2295083325147687 ) ) ;
#10859 = EDGE_LOOP ( 'NONE', ( #10331, #2352 ) ) ;
#10860 = CARTESIAN_POINT ( 'NONE',  ( 194.7500000000001705, -801.0618695410406644, -27.49999999999322498 ) ) ;
#10861 = EDGE_LOOP ( 'NONE', ( #18936, #6711 ) ) ;
#10862 = CARTESIAN_POINT ( 'NONE',  ( -4.000000000000000000, -7.806255641895631925E-15, -3.142992957459232350 ) ) ;
#10863 = CARTESIAN_POINT ( 'NONE',  ( 5.000000000000015099, 0.000000000000000000, 0.000000000000000000 ) ) ;
#10864 =( NAMED_UNIT ( * ) PLANE_ANGLE_UNIT ( ) SI_UNIT ( $, .RADIAN. ) );
#10865 = ORIENTED_EDGE ( 'NONE', *, *, #14355, .T. ) ;
#10866 = FACE_OUTER_BOUND ( 'NONE', #4212, .T. ) ;
#10867 = CARTESIAN_POINT ( 'NONE',  ( 123.1027542345830739, -1094.184478438182850, -28.88783501520646269 ) ) ;
#10868 = LINE ( 'NONE', #12813, #23090 ) ;
#10869 = CARTESIAN_POINT ( 'NONE',  ( 25.00004926070572253, -1001.642023387835820, -145.0000000000001137 ) ) ;
#10870 = DIRECTION ( 'NONE',  ( -1.000000000000000000, -0.000000000000000000, -0.000000000000000000 ) ) ;
#10871 = B_SPLINE_CURVE_WITH_KNOTS ( 'NONE', 3,
 ( #10635, #17974, #3346, #5174, #15288, #432, #15165, #22618, #12935, #20242 ),
 .UNSPECIFIED., .F., .F.,
 ( 4, 2, 2, 2, 4 ),
 ( 0.2739616238528958525, 0.3304712178896719310, 0.3869808119264479540, 0.4434904059632239770, 0.5000000000000000000 ),
 .UNSPECIFIED. ) ;
#10872 = FACE_BOUND ( 'NONE', #8146, .T. ) ;
#10873 = DIRECTION ( 'NONE',  ( 0.000000000000000000, 0.000000000000000000, 1.000000000000000000 ) ) ;
#10874 = EDGE_LOOP ( 'NONE', ( #19358, #11211, #10061, #20476 ) ) ;
#10875 = ORIENTED_EDGE ( 'NONE', *, *, #17351, .T. ) ;
#10876 = CARTESIAN_POINT ( 'NONE',  ( 24.99999999999999645, -5.982013681773172432E-16, -145.0000059999999849 ) ) ;
#10877 = CARTESIAN_POINT ( 'NONE',  ( 2.500000000000000000, 0.000000000000000000, 2.041999999999999815 ) ) ;
#10878 = ORIENTED_EDGE ( 'NONE', *, *, #2920, .F. ) ;
#10879 = DIRECTION ( 'NONE',  ( 0.000000000000000000, 0.000000000000000000, -1.000000000000000000 ) ) ;
#10880 = CYLINDRICAL_SURFACE ( 'NONE', #15707, 2.500000000000002220 ) ;
#10881 = ORIENTED_EDGE ( 'NONE', *, *, #4146, .F. ) ;
#10882 = CARTESIAN_POINT ( 'NONE',  ( 280.4976310729377360, 272.3436892194421262, 147.6188186979287025 ) ) ;
#10883 = DIRECTION ( 'NONE',  ( 0.6964005597823107463, -0.7176533009294141507, 6.982962677686266711E-15 ) ) ;
#10884 = VERTEX_POINT ( 'NONE', #7747 ) ;
#10885 = EDGE_CURVE ( 'NONE', #2113, #14636, #15127, .T. ) ;
#10886 = DIRECTION ( 'NONE',  ( -0.000000000000000000, -0.000000000000000000, 1.000000000000000000 ) ) ;
#10887 = FACE_OUTER_BOUND ( 'NONE', #15008, .T. ) ;
#10888 = ORIENTED_EDGE ( 'NONE', *, *, #14712, .F. ) ;
#10889 = EDGE_CURVE ( 'NONE', #16985, #5348, #9801, .T. ) ;
#10890 = LINE ( 'NONE', #11246, #13061 ) ;
#10891 = CARTESIAN_POINT ( 'NONE',  ( -135.8686487629346402, -1074.597166325825810, 32.50000000000645883 ) ) ;
#10892 = DIRECTION ( 'NONE',  ( 0.000000000000000000, 0.000000000000000000, 1.000000000000000000 ) ) ;
#10893 = ORIENTED_EDGE ( 'NONE', *, *, #11367, .T. ) ;
#10894 = VERTEX_POINT ( 'NONE', #22456 ) ;
#10895 = CARTESIAN_POINT ( 'NONE',  ( 7.894787914004607998, 0.7661396099416312166, -7.591390474663430865 ) ) ;
#10896 = DIRECTION ( 'NONE',  ( 1.221966984364620947E-29, 3.495664435217746987E-15, -1.000000000000000000 ) ) ;
#10897 = CARTESIAN_POINT ( 'NONE',  ( -126.8186628169058139, 89.11812652456539752, -31.65816015360259428 ) ) ;
#10898 = LINE ( 'NONE', #16309, #1098 ) ;
#10899 = LINE ( 'NONE', #21961, #8214 ) ;
#10900 = B_SPLINE_CURVE_WITH_KNOTS ( 'NONE', 3,
 ( #15975, #4408, #23319, #21510, #14878, #11032, #5451, #10797, #3384, #22211, #5563, #16792, #16563, #21989, #18588, #12973, #9327, #23673, #16681, #10917, #11279, #1937, #18140, #20280, #22092, #12861, #1588, #13096 ),
 .UNSPECIFIED., .F., .F.,
 ( 4, 2, 2, 2, 2, 2, 2, 2, 2, 2, 2, 2, 2, 4 ),
 ( 0.007862850516742106791, 0.008354729399060536327, 0.008846608281378965863, 0.009830366046016317597, 0.01032224492833499346, 0.01081412381065366933, 0.01130600269297234520, 0.01179788157529102106, 0.01278163933992838147, 0.01327351822224696887, 0.01376539710456555453, 0.01425727598688414019, 0.01474915486920272412, 0.01573291263383936808 ),
 .UNSPECIFIED. ) ;
#10901 = ORIENTED_EDGE ( 'NONE', *, *, #5722, .T. ) ;
#10902 = CARTESIAN_POINT ( 'NONE',  ( 2.500000000000000000, 3.004629197474318851E-15, 2.042000000000000259 ) ) ;
#10903 = ADVANCED_FACE ( 'NONE', ( #8222 ), #10056, .F. ) ;
#10904 = DIRECTION ( 'NONE',  ( 3.469446951953614682E-16, -1.000000000000000000, 3.483493295888648978E-15 ) ) ;
#10905 = EDGE_CURVE ( 'NONE', #16143, #9210, #7295, .T. ) ;
#10906 = DIRECTION ( 'NONE',  ( -1.000000000000000000, 7.709882115452476934E-17, 0.000000000000000000 ) ) ;
#10907 = ORIENTED_EDGE ( 'NONE', *, *, #19759, .T. ) ;
#10908 = DIRECTION ( 'NONE',  ( 2.238759164535664589E-46, 3.469446951953614189E-15, 1.000000000000000000 ) ) ;
#10910 = ADVANCED_FACE ( 'NONE', ( #22572 ), #18701, .F. ) ;
#10909 = VERTEX_POINT ( 'NONE', #15239 ) ;
#10911 = DIRECTION ( 'NONE',  ( 1.000000000000000000, 0.000000000000000000, 0.000000000000000000 ) ) ;
#10912 = VERTEX_POINT ( 'NONE', #844 ) ;
#10913 = LINE ( 'NONE', #9197, #3067 ) ;
#10914 = CARTESIAN_POINT ( 'NONE',  ( 18.83467029480908650, -1016.520668764518064, 145.0000119999999697 ) ) ;
#10915 = ADVANCED_FACE ( 'NONE', ( #15601 ), #20896, .F. ) ;
#10916 = DIRECTION ( 'NONE',  ( 1.000000000000000000, 0.000000000000000000, 0.000000000000000000 ) ) ;
#10917 = CARTESIAN_POINT ( 'NONE',  ( 125.6594390352173463, -1090.745324718712482, -31.52881987646419404 ) ) ;
#10918 = FACE_OUTER_BOUND ( 'NONE', #461, .T. ) ;
#10919 = EDGE_LOOP ( 'NONE', ( #20212, #19671, #21060, #22883 ) ) ;
#10920 = CARTESIAN_POINT ( 'NONE',  ( 140.0355749532205891, 37.61698748598766429, -90.00000000000000000 ) ) ;
#10921 = AXIS2_PLACEMENT_3D ( 'NONE', #5775, #18431, #18212 ) ;
#10923 = VERTEX_POINT ( 'NONE', #22927 ) ;
#10922 = ORIENTED_EDGE ( 'NONE', *, *, #12689, .F. ) ;
#10924 = DIRECTION ( 'NONE',  ( 1.000000000000000000, -3.495664435217746987E-15, 0.000000000000000000 ) ) ;
#10925 = CARTESIAN_POINT ( 'NONE',  ( 144.8060344827585482, 7.497491405673236464, 90.00000000000000000 ) ) ;
#10926 = CARTESIAN_POINT ( 'NONE',  ( 4.000000000000000000, 0.7924765000094659007, -0.05906175389889852662 ) ) ;
#10927 = ORIENTED_EDGE ( 'NONE', *, *, #22537, .F. ) ;
#10928 = AXIS2_PLACEMENT_3D ( 'NONE', #9297, #23757, #14603 ) ;
#10929 = LINE ( 'NONE', #23580, #259 ) ;
#10930 = CARTESIAN_POINT ( 'NONE',  ( -2.700000000000001066, 0.000000000000000000, -25.00000000000000000 ) ) ;
#10931 = VERTEX_POINT ( 'NONE', #4229 ) ;
#10932 = EDGE_CURVE ( 'NONE', #20062, #2118, #21965, .T. ) ;
#10933 = EDGE_CURVE ( 'NONE', #13544, #15472, #16194, .T. ) ;
#10934 = DIRECTION ( 'NONE',  ( 0.000000000000000000, 0.000000000000000000, 1.000000000000000000 ) ) ;
#10935 = DIRECTION ( 'NONE',  ( 6.753181414994864868E-15, 0.000000000000000000, -1.000000000000000000 ) ) ;
#10936 = VERTEX_POINT ( 'NONE', #5389 ) ;
#10937 = AXIS2_PLACEMENT_3D ( 'NONE', #14286, #21488, #6403 ) ;
#10938 = ORIENTED_EDGE ( 'NONE', *, *, #23482, .F. ) ;
#10939 = DIRECTION ( 'NONE',  ( 0.000000000000000000, 0.000000000000000000, -1.000000000000000000 ) ) ;
#10940 = ORIENTED_EDGE ( 'NONE', *, *, #5772, .F. ) ;
#10941 = CARTESIAN_POINT ( 'NONE',  ( -128.6141261030697649, 86.50721885637406672, 32.18904844917290831 ) ) ;
#10942 = ADVANCED_FACE ( 'NONE', ( #22392 ), #21196, .F. ) ;
#10943 = LINE ( 'NONE', #5243, #12734 ) ;
#10944 = CARTESIAN_POINT ( 'NONE',  ( -285.2000000000011255, -29.99999999999898037, -105.0000000000000000 ) ) ;
#10945 = EDGE_CURVE ( 'NONE', #1156, #7096, #14813, .T. ) ;
#10946 = DIRECTION ( 'NONE',  ( 1.000000000000000000, 2.775557561562891351E-17, 0.000000000000000000 ) ) ;
#10947 = CARTESIAN_POINT ( 'NONE',  ( -2.999999999999995559, 2.632990618166809235E-15, 21.50000000000000000 ) ) ;
#10948 =( NAMED_UNIT ( * ) PLANE_ANGLE_UNIT ( ) SI_UNIT ( $, .RADIAN. ) );
#10949 = EDGE_LOOP ( 'NONE', ( #7844, #813, #13042, #3493 ) ) ;
#10950 = EDGE_CURVE ( 'NONE', #12413, #3845, #18399, .T. ) ;
#10951 = SURFACE_STYLE_FILL_AREA ( #13009 ) ;
#10952 = DIRECTION ( 'NONE',  ( 0.000000000000000000, 0.000000000000000000, -1.000000000000000000 ) ) ;
#10953 = LINE ( 'NONE', #18275, #3089 ) ;
#10954 = AXIS2_PLACEMENT_3D ( 'NONE', #10020, #23019, #13907 ) ;
#10955 =( REPRESENTATION_RELATIONSHIP ('NONE','NONE', #10127, #18083 ) REPRESENTATION_RELATIONSHIP_WITH_TRANSFORMATION ( #9605 )SHAPE_REPRESENTATION_RELATIONSHIP( ) );
#10956 = EDGE_LOOP ( 'NONE', ( #22582, #2774, #688, #1092 ) ) ;
#10957 = CARTESIAN_POINT ( 'NONE',  ( 281.4928932188133786, -127.0000000000000568, 150.2000000000013813 ) ) ;
#10958 = LINE ( 'NONE', #22029, #21899 ) ;
#10959 = CARTESIAN_POINT ( 'NONE',  ( 7.342598717236928252, 0.000000000000000000, 0.000000000000000000 ) ) ;
#10960 = CARTESIAN_POINT ( 'NONE',  ( 0.000000000000000000, 0.000000000000000000, 90.00000000000000000 ) ) ;
#10961 = CARTESIAN_POINT ( 'NONE',  ( 280.2494876630255476, 272.8327955282143193, -146.3518577254344564 ) ) ;
#10962 = VERTEX_POINT ( 'NONE', #22144 ) ;
#10964 = DIRECTION ( 'NONE',  ( -1.000000000000000000, -0.000000000000000000, -0.000000000000000000 ) ) ;
#10963 = CONICAL_SURFACE ( 'NONE', #13691, 2.041999999999999815, 1.047197551196591858 ) ;
#10965 = EDGE_LOOP ( 'NONE', ( #19461, #22408, #21655, #12171 ) ) ;
#10966 = FACE_OUTER_BOUND ( 'NONE', #195, .T. ) ;
#10967 = AXIS2_PLACEMENT_3D ( 'NONE', #15266, #2792, #10183 ) ;
#10968 = EDGE_CURVE ( 'NONE', #9681, #20782, #15623, .T. ) ;
#10969 = CARTESIAN_POINT ( 'NONE',  ( -31.74999999999995737, 0.000000000000000000, 0.000000000000000000 ) ) ;
#10970 = EDGE_CURVE ( 'NONE', #18161, #7547, #16387, .T. ) ;
#10971 = VERTEX_POINT ( 'NONE', #3785 ) ;
#10972 =( LENGTH_UNIT ( ) NAMED_UNIT ( * ) SI_UNIT ( .MILLI., .METRE. ) );
#10973 = CARTESIAN_POINT ( 'NONE',  ( 123.9851406373740446, -1093.019934698474344, -32.37389708099357932 ) ) ;
#10974 = EDGE_CURVE ( 'NONE', #17846, #9561, #15581, .T. ) ;
#10975 = CARTESIAN_POINT ( 'NONE',  ( 146.4450000000002490, -210.0000000000003411, -32.49999999999356248 ) ) ;
#10976 = CARTESIAN_POINT ( 'NONE',  ( 24.83992656992418446, -1003.266860234099909, -145.0000000000001421 ) ) ;
#10977 = EDGE_CURVE ( 'NONE', #20656, #4421, #3553, .T. ) ;
#10978 = CARTESIAN_POINT ( 'NONE',  ( 2.500000000000000000, 0.000000000000000000, 0.000000000000000000 ) ) ;
#10979 = CARTESIAN_POINT ( 'NONE',  ( -72.64999999999996305, -87.33333333333338544, 124.9999999999999858 ) ) ;
#10980 = CARTESIAN_POINT ( 'NONE',  ( -8.055391459054618508, 23.72315261474503600, 145.0000119999999697 ) ) ;
#10981 = VERTEX_POINT ( 'NONE', #18753 ) ;
#10982 = EDGE_CURVE ( 'NONE', #22508, #3871, #437, .T. ) ;
#10983 = ORIENTED_EDGE ( 'NONE', *, *, #23208, .F. ) ;
#10984 = CARTESIAN_POINT ( 'NONE',  ( -45.00000000000000000, 272.9999999999999432, 0.000000000000000000 ) ) ;
#10985 = CARTESIAN_POINT ( 'NONE',  ( 0.000000000000000000, 0.000000000000000000, 150.0000000000000284 ) ) ;
#10986 = EDGE_CURVE ( 'NONE', #2402, #13198, #11785, .T. ) ;
#10987 = VERTEX_POINT ( 'NONE', #12907 ) ;
#10988 = PRODUCT ( 'socket head cap screw_iso_ISO 4762 M5 x 12 - 12N', 'socket head cap screw_iso_ISO 4762 M5 x 12 - 12N', '', ( #9304 ) ) ;
#10989 = CARTESIAN_POINT ( 'NONE',  ( 0.000000000000000000, -132.2000000000000455, -177.2000000000013529 ) ) ;
#10991 =( GEOMETRIC_REPRESENTATION_CONTEXT ( 3 ) GLOBAL_UNCERTAINTY_ASSIGNED_CONTEXT ( ( #11901 ) ) GLOBAL_UNIT_ASSIGNED_CONTEXT ( ( #18586, #1935, #9433 ) ) REPRESENTATION_CONTEXT ( 'NONE', 'WORKASPACE' ) );
#10990 = CARTESIAN_POINT ( 'NONE',  ( 0.000000000000000000, -1000.000000000000000, 138.9999999999999716 ) ) ;
#10992 = ORIENTED_EDGE ( 'NONE', *, *, #9111, .F. ) ;
#10993 = CARTESIAN_POINT ( 'NONE',  ( 119.6158142514525480, -1087.367367941136990, -27.94499999999356987 ) ) ;
#10994 = CARTESIAN_POINT ( 'NONE',  ( 135.4018704341561374, -51.87806360044677234, -90.00000000000000000 ) ) ;
#10995 = EDGE_LOOP ( 'NONE', ( #12555, #17572, #8960, #5945 ) ) ;
#10996 = CARTESIAN_POINT ( 'NONE',  ( 232.0000000000000284, -2.031704083844970052E-14, 57.00000000000024869 ) ) ;
#10997 = CARTESIAN_POINT ( 'NONE',  ( 7.922281120364393914, 4.573931137438269623, -8.047472243342930653 ) ) ;
#10998 = CARTESIAN_POINT ( 'NONE',  ( -281.4928932188135491, -132.2000000000000455, 177.2000000000014097 ) ) ;
#10999 = ORIENTED_EDGE ( 'NONE', *, *, #6154, .T. ) ;
#11000 = CARTESIAN_POINT ( 'NONE',  ( -155.0000000000000284, -494.4690652294799520, -29.99999999999350564 ) ) ;
#11001 = CARTESIAN_POINT ( 'NONE',  ( -136.5850230665614902, -1073.277182683704496, 31.88926668738024262 ) ) ;
#11002 = FACE_OUTER_BOUND ( 'NONE', #15954, .T. ) ;
#11003 = VERTEX_POINT ( 'NONE', #9372 ) ;
#11004 = ORIENTED_EDGE ( 'NONE', *, *, #2382, .T. ) ;
#11005 = FACE_OUTER_BOUND ( 'NONE', #12267, .T. ) ;
#11006 = VECTOR ( 'NONE', #3668, 1000.000000000000000 ) ;
#11007 = APPLICATION_PROTOCOL_DEFINITION ( 'draft international standard', 'automotive_design', 1998, #10639 ) ;
#11008 = CARTESIAN_POINT ( 'NONE',  ( 0.000000000000000000, 0.000000000000000000, 90.00000000000000000 ) ) ;
#11009 = CIRCLE ( 'NONE', #17513, 2.041999999999999815 ) ;
#11010 = CARTESIAN_POINT ( 'NONE',  ( 45.00000000000002132, -52.79999999999936477, 140.0000000000001990 ) ) ;
#11011 = CARTESIAN_POINT ( 'NONE',  ( 3.999999999999999112, -0.7890432684750902093, -0.04868663549882291247 ) ) ;
#11012 = CIRCLE ( 'NONE', #19066, 2.649999999999971934 ) ;
#11013 = ORIENTED_EDGE ( 'NONE', *, *, #17522, .T. ) ;
#11014 = ADVANCED_FACE ( 'NONE', ( #3910 ), #7540, .F. ) ;
#11015 = CARTESIAN_POINT ( 'NONE',  ( -19.87769063953886217, -15.24974479720506970, 145.0000119999999981 ) ) ;
#11016 = EDGE_CURVE ( 'NONE', #17622, #9308, #2716, .T. ) ;
#11017 = PRODUCT_DEFINITION_CONTEXT ( 'detailed design', #19547, 'design' ) ;
#11018 = LINE ( 'NONE', #3719, #22911 ) ;
#11019 = CARTESIAN_POINT ( 'NONE',  ( 2.699999999999997513, 0.000000000000000000, 0.000000000000000000 ) ) ;
#11020 = ORIENTED_EDGE ( 'NONE', *, *, #17842, .T. ) ;
#11021 = CARTESIAN_POINT ( 'NONE',  ( -2.352990130084580066E-16, 8.660254037844390851, -7.422398894150034288 ) ) ;
#11022 = AXIS2_PLACEMENT_3D ( 'NONE', #11496, #17148, #19059 ) ;
#11023 = CLOSED_SHELL ( 'NONE', ( #22089, #17418, #5593, #20988, #7260, #2378, #2773, #7518, #5435, #7473, #10855, #17566, #5203, #21279, #7522, #5290, #4376, #3245, #19834, #14448, #12255, #325, #10903, #138, #8081, #18891, #11383, #3248, #23308, #13174, #4731, #10707, #7482, #4848, #16249, #19964 ) ) ;
#11024 = ORIENTED_EDGE ( 'NONE', *, *, #6803, .T. ) ;
#11025 = CYLINDRICAL_SURFACE ( 'NONE', #11022, 9.999999999999998224 ) ;
#11026 = CARTESIAN_POINT ( 'NONE',  ( 0.02511973781850649831, -4.877415612947427981, -3.751298745799844792 ) ) ;
#11027 = ORIENTED_EDGE ( 'NONE', *, *, #23695, .F. ) ;
#11028 = CARTESIAN_POINT ( 'NONE',  ( 17.00000000000000000, 0.000000000000000000, 0.000000000000000000 ) ) ;
#11029 = AXIS2_PLACEMENT_3D ( 'NONE', #8130, #17416, #23062 ) ;
#11030 = DIRECTION ( 'NONE',  ( 0.000000000000000000, 0.000000000000000000, -1.000000000000000000 ) ) ;
#11031 = CARTESIAN_POINT ( 'NONE',  ( -158.1195828810602109, 116.4077317428687621, -29.99999999999322498 ) ) ;
#11032 = CARTESIAN_POINT ( 'NONE',  ( 125.2216071840745997, -1091.349008980712597, -27.81095155082704906 ) ) ;
#11033 = CARTESIAN_POINT ( 'NONE',  ( -56.99999999999995737, -56.80000000000003268, 5.199999999999971756 ) ) ;
#11034 = EDGE_LOOP ( 'NONE', ( #19208, #13941 ) ) ;
#11035 = DIRECTION ( 'NONE',  ( 0.6964005597823107463, -0.7176533009294141507, 6.982962677686266711E-15 ) ) ;
#11036 = FACE_BOUND ( 'NONE', #8434, .T. ) ;
#11037 = AXIS2_PLACEMENT_3D ( 'NONE', #9542, #9790, #7967 ) ;
#11039 = ORIENTED_EDGE ( 'NONE', *, *, #17933, .T. ) ;
#11038 = ORIENTED_EDGE ( 'NONE', *, *, #18749, .T. ) ;
#11040 = AXIS2_PLACEMENT_3D ( 'NONE', #23166, #13681, #15934 ) ;
#11041 = DIRECTION ( 'NONE',  ( 1.000000000000000000, 0.000000000000000000, 0.000000000000000000 ) ) ;
#11042 = CARTESIAN_POINT ( 'NONE',  ( -64.99999999999998579, -56.79999999999943583, 125.0000000000001705 ) ) ;
#11043 = CARTESIAN_POINT ( 'NONE',  ( 0.000000000000000000, 0.000000000000000000, -50.00000000000000000 ) ) ;
#11044 = VERTEX_POINT ( 'NONE', #15409 ) ;
#11045 = CARTESIAN_POINT ( 'NONE',  ( -40.00000000000000000, 100.0000000000000000, 150.2000000000009550 ) ) ;
#11046 = CIRCLE ( 'NONE', #22964, 7.500000000000000888 ) ;
#11047 = PLANE ( 'NONE',  #21119 ) ;
#11048 = ORIENTED_EDGE ( 'NONE', *, *, #9357, .T. ) ;
#11049 = AXIS2_PLACEMENT_3D ( 'NONE', #11139, #18464, #1923 ) ;
#11050 = DIRECTION ( 'NONE',  ( 0.000000000000000000, 0.000000000000000000, 1.000000000000000000 ) ) ;
#11051 = DIRECTION ( 'NONE',  ( -1.000000000000000000, -0.000000000000000000, -0.000000000000000000 ) ) ;
#11052 = ITEM_DEFINED_TRANSFORMATION ( 'NONE', 'NONE', #6958,  #11210 ) ;
#11053 = ORIENTED_EDGE ( 'NONE', *, *, #2615, .T. ) ;
#11054 = AXIS2_PLACEMENT_3D ( 'NONE', #662, #22763, #2719 ) ;
#11055 = CARTESIAN_POINT ( 'NONE',  ( 125.7677891478060417, -1090.595098045220539, 28.74299381080691873 ) ) ;
#11056 = VERTEX_POINT ( 'NONE', #22760 ) ;
#11057 = CARTESIAN_POINT ( 'NONE',  ( -129.3180659214442301, 85.45079184243522263, 29.67150201188731984 ) ) ;
#11058 = CARTESIAN_POINT ( 'NONE',  ( 134.0925202534283756, 77.74453171555596498, 29.33965772977898467 ) ) ;
#11059 = CARTESIAN_POINT ( 'NONE',  ( 4.000000000000000000, 1.680228229147133767, -3.316631783032546021 ) ) ;
#11060 = DIRECTION ( 'NONE',  ( 8.144298233840332611E-17, 3.483493295888648978E-15, 1.000000000000000000 ) ) ;
#11061 = LINE ( 'NONE', #18516, #5364 ) ;
#11062 = AXIS2_PLACEMENT_3D ( 'NONE', #22495, #2452, #20682 ) ;
#11063 = FACE_OUTER_BOUND ( 'NONE', #9579, .T. ) ;
#11064 = EDGE_LOOP ( 'NONE', ( #15448, #5119 ) ) ;
#11065 = EDGE_CURVE ( 'NONE', #4477, #16985, #2817, .T. ) ;
#11066 = DIRECTION ( 'NONE',  ( -1.000000000000000000, 0.000000000000000000, -6.982962677686266711E-15 ) ) ;
#11067 = DIRECTION ( 'NONE',  ( 0.000000000000000000, 0.000000000000000000, 1.000000000000000000 ) ) ;
#11068 = CARTESIAN_POINT ( 'NONE',  ( 7.894787914004607998, 1.243647571710251278E-13, -7.591390474663425536 ) ) ;
#11069 = EDGE_CURVE ( 'NONE', #2779, #10987, #4651, .T. ) ;
#11070 = EDGE_CURVE ( 'NONE', #16653, #3521, #4018, .T. ) ;
#11071 = ORIENTED_EDGE ( 'NONE', *, *, #15826, .T. ) ;
#11072 = CARTESIAN_POINT ( 'NONE',  ( 281.0571594757293497, 268.7755899421583763, -146.9771650631952582 ) ) ;
#11073 = DIRECTION ( 'NONE',  ( 0.000000000000000000, -2.618450529776326854E-15, -1.000000000000000000 ) ) ;
#11074 = EDGE_CURVE ( 'NONE', #13966, #16206, #9974, .T. ) ;
#11075 = DIRECTION ( 'NONE',  ( 0.000000000000000000, 0.000000000000000000, 1.000000000000000000 ) ) ;
#11076 = CYLINDRICAL_SURFACE ( 'NONE', #4166, 7.500000000000007105 ) ;
#11077 = PLANE ( 'NONE',  #9260 ) ;
#11078 = CARTESIAN_POINT ( 'NONE',  ( 0.000000000000000000, 5.068713431065764784E-13, -147.2000000000008981 ) ) ;
#11079 = ORIENTED_EDGE ( 'NONE', *, *, #11854, .F. ) ;
#11080 = CARTESIAN_POINT ( 'NONE',  ( -12.52876685377503385, -978.3042100244115318, 145.0000119999999697 ) ) ;
#11081 = VERTEX_POINT ( 'NONE', #2461 ) ;
#11082 = CARTESIAN_POINT ( 'NONE',  ( -69.99999999999997158, -112.6666666666667140, 0.000000000000000000 ) ) ;
#11083 = DIRECTION ( 'NONE',  ( 0.000000000000000000, 0.000000000000000000, 1.000000000000000000 ) ) ;
#11084 = ORIENTED_EDGE ( 'NONE', *, *, #2032, .F. ) ;
#11085 = FACE_OUTER_BOUND ( 'NONE', #6930, .T. ) ;
#11086 = CARTESIAN_POINT ( 'NONE',  ( 124.0796955067752521, -1092.893784429268635, -27.57920702976965543 ) ) ;
#11087 = CARTESIAN_POINT ( 'NONE',  ( -0.6249999999999991118, -8.299410119600880265, -7.298562697733108173 ) ) ;
#11088 = CARTESIAN_POINT ( 'NONE',  ( 194.7500000000001990, -801.0618695410406644, -29.99999999999322498 ) ) ;
#11089 = CARTESIAN_POINT ( 'NONE',  ( -5.560781378645575757, 6.809993116116508640E-16, -4.000000000000000000 ) ) ;
#11090 = DIRECTION ( 'NONE',  ( 0.000000000000000000, 0.000000000000000000, 1.000000000000000000 ) ) ;
#11091 = AXIS2_PLACEMENT_3D ( 'NONE', #12124, #18449, #16313 ) ;
#11092 = CARTESIAN_POINT ( 'NONE',  ( 19.87769063953886217, 15.24974479720507325, 145.0000119999999981 ) ) ;
#11093 = APPLICATION_CONTEXT ( 'automotive_design' ) ;
#11094 = VERTEX_POINT ( 'NONE', #11931 ) ;
#11095 = ORIENTED_EDGE ( 'NONE', *, *, #7628, .T. ) ;
#11096 = CARTESIAN_POINT ( 'NONE',  ( 0.3208286057739604957, -4.433571671609698228, -0.3503314178412692548 ) ) ;
#11097 = CIRCLE ( 'NONE', #20711, 7.500000000000001776 ) ;
#11098 = DIRECTION ( 'NONE',  ( -0.5000000000000051070, 0.000000000000000000, 0.8660254037844355990 ) ) ;
#11099 = EDGE_LOOP ( 'NONE', ( #20644, #1189, #18156, #10066 ) ) ;
#11100 = EDGE_CURVE ( 'NONE', #20023, #17062, #15646, .T. ) ;
#11101 = CARTESIAN_POINT ( 'NONE',  ( 9.999999999999998224, 1.183533879463814165, 200.0000119999999697 ) ) ;
#11102 = CARTESIAN_POINT ( 'NONE',  ( 7.970070017554212960, -4.546953124339766283, -8.057670357645358550 ) ) ;
#11103 = ADVANCED_FACE ( 'NONE', ( #20691 ), #6221, .F. ) ;
#11104 = ORIENTED_EDGE ( 'NONE', *, *, #3119, .T. ) ;
#11105 = FACE_OUTER_BOUND ( 'NONE', #3391, .T. ) ;
#11106 = EDGE_CURVE ( 'NONE', #13119, #8023, #2868, .T. ) ;
#11107 = CARTESIAN_POINT ( 'NONE',  ( -3.333333333333335258, 2.694301256218251783, -3.300726591567079815 ) ) ;
#11108 = ORIENTED_EDGE ( 'NONE', *, *, #14124, .T. ) ;
#11109 = DIRECTION ( 'NONE',  ( 0.000000000000000000, -2.618450529776326854E-15, -1.000000000000000000 ) ) ;
#11110 = CARTESIAN_POINT ( 'NONE',  ( 1.306442393143578906, 8.377108146505383601, -7.792327460285857654 ) ) ;
#11111 = AXIS2_PLACEMENT_3D ( 'NONE', #3951, #11364, #8206 ) ;
#11112 = ADVANCED_FACE ( 'NONE', ( #886 ), #946, .F. ) ;
#11113 = LINE ( 'NONE', #9518, #3822 ) ;
#11114 = ORIENTED_EDGE ( 'NONE', *, *, #10763, .T. ) ;
#11115 = DIRECTION ( 'NONE',  ( -1.000000000000000000, 0.000000000000000000, 0.000000000000000000 ) ) ;
#11117 = CARTESIAN_POINT ( 'NONE',  ( -136.9597779064867780, -1072.574344195404137, 29.33965772977902731 ) ) ;
#11116 = PRODUCT_RELATED_PRODUCT_CATEGORY ( 'part', '', ( #15766 ) ) ;
#11118 = AXIS2_PLACEMENT_3D ( 'NONE', #11559, #9602, #22853 ) ;
#11119 = LINE ( 'NONE', #470, #3217 ) ;
#11120 = AXIS2_PLACEMENT_3D ( 'NONE', #1040, #8424, #3326 ) ;
#11121 = VERTEX_POINT ( 'NONE', #15171 ) ;
#11122 = ORIENTED_EDGE ( 'NONE', *, *, #22293, .F. ) ;
#11123 = DIRECTION ( 'NONE',  ( 0.000000000000000000, -1.000000000000000000, 0.000000000000000000 ) ) ;
#11124 = APPLICATION_PROTOCOL_DEFINITION ( 'draft international standard', 'automotive_design', 1998, #7209 ) ;
#11125 = CARTESIAN_POINT ( 'NONE',  ( -127.1840658299259417, 88.59589253999689618, -27.82770220384454518 ) ) ;
#11126 = CARTESIAN_POINT ( 'NONE',  ( 40.00000000000000000, 100.0000000000000000, 150.2000000000009550 ) ) ;
#11127 = FACE_BOUND ( 'NONE', #17862, .T. ) ;
#11128 = ORIENTED_EDGE ( 'NONE', *, *, #4602, .F. ) ;
#11129 = CARTESIAN_POINT ( 'NONE',  ( -146.0000000000005400, -494.4690652294800657, -32.05499999999356930 ) ) ;
#11130 = VECTOR ( 'NONE', #17819, 1000.000000000000000 ) ;
#11131 = AXIS2_PLACEMENT_3D ( 'NONE', #7266, #14540, #21874 ) ;
#11132 = AXIS2_PLACEMENT_3D ( 'NONE', #23353, #13988, #19728 ) ;
#11133 = UNCERTAINTY_MEASURE_WITH_UNIT (LENGTH_MEASURE( 1.000000000000000082E-05 ), #12242, 'distance_accuracy_value', 'NONE');
#11134 = DIRECTION ( 'NONE',  ( -1.000000000000000000, -9.912705577010325549E-17, -3.465149234233960866E-31 ) ) ;
#11135 = AXIS2_PLACEMENT_3D ( 'NONE', #6179, #16166, #19772 ) ;
#11136 = DIRECTION ( 'NONE',  ( 0.000000000000000000, 0.000000000000000000, 1.000000000000000000 ) ) ;
#11137 = ORIENTED_EDGE ( 'NONE', *, *, #14052, .T. ) ;
#11138 =( REPRESENTATION_RELATIONSHIP ('NONE','NONE', #10127, #11474 ) REPRESENTATION_RELATIONSHIP_WITH_TRANSFORMATION ( #15262 )SHAPE_REPRESENTATION_RELATIONSHIP( ) );
#11139 = CARTESIAN_POINT ( 'NONE',  ( -2.699999999999995737, 2.486033002269127373E-15, 20.30000000000000071 ) ) ;
#11140 = ORIENTED_EDGE ( 'NONE', *, *, #3434, .F. ) ;
#11141 = EDGE_CURVE ( 'NONE', #13958, #17412, #13628, .T. ) ;
#11142 = EDGE_CURVE ( 'NONE', #13673, #11044, #13740, .T. ) ;
#11143 = CARTESIAN_POINT ( 'NONE',  ( 49.17200000000001836, 6.123233995736769241E-16, -5.000000000000002665 ) ) ;
#11144 = EDGE_CURVE ( 'NONE', #11951, #7507, #14423, .T. ) ;
#11145 = CARTESIAN_POINT ( 'NONE',  ( -127.9021285790837510, 87.55595642181941685, -32.49999999999351985 ) ) ;
#11146 = ORIENTED_EDGE ( 'NONE', *, *, #21854, .F. ) ;
#11147 = CARTESIAN_POINT ( 'NONE',  ( -2.621086668468698644, -7.606368536631371136, -7.634085501268427443 ) ) ;
#11148 = CARTESIAN_POINT ( 'NONE',  ( -110.0000000000000000, -94.99999999999997158, 0.000000000000000000 ) ) ;
#11149 = AXIS2_PLACEMENT_3D ( 'NONE', #10085, #23201, #11783 ) ;
#11150 = AXIS2_PLACEMENT_3D ( 'NONE', #10125, #8540, #17580 ) ;
#11151 = CARTESIAN_POINT ( 'NONE',  ( 5.000000000000000888, 4.250000000000000000, 0.000000000000000000 ) ) ;
#11152 = CIRCLE ( 'NONE', #11944, 2.649999999999985700 ) ;
#11153 = CARTESIAN_POINT ( 'NONE',  ( -280.9755403010747159, 269.7771302778487552, -145.4357197208657055 ) ) ;
#11154 = CARTESIAN_POINT ( 'NONE',  ( 4.336808689942017736E-16, 8.660254037844390851, -1.000000000000000888 ) ) ;
#11155 = CIRCLE ( 'NONE', #14986, 20.00000000000000000 ) ;
#11156 = DIRECTION ( 'NONE',  ( 0.000000000000000000, -0.000000000000000000, 1.000000000000000000 ) ) ;
#11157 = ORIENTED_EDGE ( 'NONE', *, *, #8544, .T. ) ;
#11158 = CARTESIAN_POINT ( 'NONE',  ( 0.000000000000000000, 0.000000000000000000, 100.0000000000000000 ) ) ;
#11159 = CARTESIAN_POINT ( 'NONE',  ( -4.250000000000000000, 5.204748896376250699E-16, -10.00000000000000000 ) ) ;
#11161 = EDGE_LOOP ( 'NONE', ( #16441, #7922, #11468, #11122 ) ) ;
#11160 = VERTEX_POINT ( 'NONE', #4397 ) ;
#11162 = DIRECTION ( 'NONE',  ( 1.224646799147353207E-16, -4.064521778635712183E-50, -1.000000000000000000 ) ) ;
#11163 = CARTESIAN_POINT ( 'NONE',  ( -136.1785371930675410, -1074.029921987504395, -27.62591505085369903 ) ) ;
#11164 = CARTESIAN_POINT ( 'NONE',  ( 281.3684665479255500, 268.0880230824753312, -147.1999999999999318 ) ) ;
#11165 = ORIENTED_EDGE ( 'NONE', *, *, #7102, .F. ) ;
#11166 = AXIS2_PLACEMENT_3D ( 'NONE', #3945, #13416, #18792 ) ;
#11167 = CARTESIAN_POINT ( 'NONE',  ( -135.7102838464026036, -1074.884883977198115, 32.50000000000647304 ) ) ;
#11169 = CIRCLE ( 'NONE', #2245, 2.649999999999971934 ) ;
#11168 =( GEOMETRIC_REPRESENTATION_CONTEXT ( 3 ) GLOBAL_UNCERTAINTY_ASSIGNED_CONTEXT ( ( #11133 ) ) GLOBAL_UNIT_ASSIGNED_CONTEXT ( ( #12242, #12376, #6527 ) ) REPRESENTATION_CONTEXT ( 'NONE', 'WORKASPACE' ) );
#11170 = ORIENTED_EDGE ( 'NONE', *, *, #3725, .F. ) ;
#11171 = CIRCLE ( 'NONE', #722, 2.649999999999971934 ) ;
#11172 = CIRCLE ( 'NONE', #7669, 2.649999999999971934 ) ;
#11173 = DIRECTION ( 'NONE',  ( 0.000000000000000000, 0.000000000000000000, 1.000000000000000000 ) ) ;
#11174 = VECTOR ( 'NONE', #15387, 1000.000000000000000 ) ;
#11175 = ORIENTED_EDGE ( 'NONE', *, *, #17644, .F. ) ;
#11176 = EDGE_CURVE ( 'NONE', #22022, #12343, #13857, .T. ) ;
#11177 = CARTESIAN_POINT ( 'NONE',  ( 0.000000000000000000, 0.000000000000000000, -90.00000000000000000 ) ) ;
#11178 = LINE ( 'NONE', #16702, #16937 ) ;
#11179 = AXIS2_PLACEMENT_3D ( 'NONE', #18063, #23609, #10240 ) ;
#11180 = CONTEXT_DEPENDENT_SHAPE_REPRESENTATION ( #3231, #13765 ) ;
#11181 = VERTEX_POINT ( 'NONE', #2347 ) ;
#11182 = ADVANCED_FACE ( 'NONE', ( #6330 ), #12064, .F. ) ;
#11183 = CARTESIAN_POINT ( 'NONE',  ( 125.8877979345646736, -1090.428239381491267, 30.81384172145508771 ) ) ;
#11184 = VERTEX_POINT ( 'NONE', #19357 ) ;
#11185 = CYLINDRICAL_SURFACE ( 'NONE', #9394, 2.500000000000002220 ) ;
#11186 = DIRECTION ( 'NONE',  ( -0.000000000000000000, -0.000000000000000000, 1.000000000000000000 ) ) ;
#11187 = CARTESIAN_POINT ( 'NONE',  ( 1.393927851585479161, -4.043713361053543842, -3.526374918436840922 ) ) ;
#11188 = CONICAL_SURFACE ( 'NONE', #23495, 2.055000000000001492, 0.7853981633974633780 ) ;
#11189 = DIRECTION ( 'NONE',  ( 0.000000000000000000, -1.000000000000000000, 0.000000000000000000 ) ) ;
#11190 =( GEOMETRIC_REPRESENTATION_CONTEXT ( 3 ) GLOBAL_UNCERTAINTY_ASSIGNED_CONTEXT ( ( #20618 ) ) GLOBAL_UNIT_ASSIGNED_CONTEXT ( ( #23236, #5025, #21558 ) ) REPRESENTATION_CONTEXT ( 'NONE', 'WORKASPACE' ) );
#11191 = DIRECTION ( 'NONE',  ( 0.000000000000000000, 0.000000000000000000, 1.000000000000000000 ) ) ;
#11192 = VECTOR ( 'NONE', #14367, 1000.000000000000000 ) ;
#11193 = AXIS2_PLACEMENT_3D ( 'NONE', #23357, #10478, #23233 ) ;
#11194 = CIRCLE ( 'NONE', #16581, 2.700000000000000622 ) ;
#11195 = CIRCLE ( 'NONE', #5423, 5.384454397937118664 ) ;
#11196 = AXIS2_PLACEMENT_3D ( 'NONE', #11880, #19189, #11509 ) ;
#11197 = ORIENTED_EDGE ( 'NONE', *, *, #849, .T. ) ;
#11198 = DIRECTION ( 'NONE',  ( 0.000000000000000000, 0.000000000000000000, 1.000000000000000000 ) ) ;
#11199 = DIRECTION ( 'NONE',  ( 1.000000000000000000, 0.000000000000000000, 0.000000000000000000 ) ) ;
#11200 = CYLINDRICAL_SURFACE ( 'NONE', #20830, 21.50000000000000000 ) ;
#11201 = ORIENTED_EDGE ( 'NONE', *, *, #1470, .T. ) ;
#11202 = DIRECTION ( 'NONE',  ( -0.5114233182937452105, 0.4883095222350190001, 0.7071067811865631159 ) ) ;
#11203 = DIRECTION ( 'NONE',  ( 0.000000000000000000, 0.000000000000000000, 1.000000000000000000 ) ) ;
#11204 = ADVANCED_FACE ( 'NONE', ( #2580 ), #546, .F. ) ;
#11205 = DIRECTION ( 'NONE',  ( 0.000000000000000000, -1.000000000000000000, 0.000000000000000000 ) ) ;
#11207 = AXIS2_PLACEMENT_3D ( 'NONE', #18946, #4347, #20635 ) ;
#11206 = AXIS2_PLACEMENT_3D ( 'NONE', #6431, #4131, #9720 ) ;
#11208 = LINE ( 'NONE', #14925, #19916 ) ;
#11209 = CARTESIAN_POINT ( 'NONE',  ( -282.2000000000011255, -29.99999999999898037, -107.6499999999999631 ) ) ;
#11210 = AXIS2_PLACEMENT_3D ( 'NONE', #9473, #14914, #3769 ) ;
#11211 = ORIENTED_EDGE ( 'NONE', *, *, #20627, .T. ) ;
#11212 = AXIS2_PLACEMENT_3D ( 'NONE', #13830, #21154, #6900 ) ;
#11213 = AXIS2_PLACEMENT_3D ( 'NONE', #4786, #23722, #6965 ) ;
#11214 = CARTESIAN_POINT ( 'NONE',  ( 6.482064212728070096, -975.7995837828526646, 145.0000119999999697 ) ) ;
#11215 = ORIENTED_EDGE ( 'NONE', *, *, #19222, .F. ) ;
#11216 = CARTESIAN_POINT ( 'NONE',  ( -145.0000000000000284, -5.062647941322544249E-13, -90.00000000000000000 ) ) ;
#11217 = DIRECTION ( 'NONE',  ( -1.000000000000000000, -0.000000000000000000, -0.000000000000000000 ) ) ;
#11218 = DIRECTION ( 'NONE',  ( 0.000000000000000000, 0.000000000000000000, -1.000000000000000000 ) ) ;
#11219 = EDGE_CURVE ( 'NONE', #12822, #7386, #9064, .T. ) ;
#11220 = ORIENTED_EDGE ( 'NONE', *, *, #21014, .F. ) ;
#11221 = FACE_OUTER_BOUND ( 'NONE', #14222, .T. ) ;
#11222 = PLANE ( 'NONE',  #3758 ) ;
#11223 = CARTESIAN_POINT ( 'NONE',  ( 2.500000000000000000, -1.768423874527823569, 1.021000000000002350 ) ) ;
#11224 = CARTESIAN_POINT ( 'NONE',  ( 194.7499999999997442, -801.0618695410399823, 30.00000000000675726 ) ) ;
#11225 = CARTESIAN_POINT ( 'NONE',  ( -40.00000000000000000, 100.0000000000000000, -125.0000000000000000 ) ) ;
#11226 = EDGE_CURVE ( 'NONE', #5058, #4246, #14854, .T. ) ;
#11227 = CARTESIAN_POINT ( 'NONE',  ( 4.101954839143060028, 2.368264730582927857, -3.681130640444267854 ) ) ;
#11228 = CARTESIAN_POINT ( 'NONE',  ( -7.908219015560238319, -3.084967917785936820, -7.795665562178438535 ) ) ;
#11229 = EDGE_LOOP ( 'NONE', ( #9996, #4087 ) ) ;
#11230 = AXIS2_PLACEMENT_3D ( 'NONE', #18221, #21622, #3135 ) ;
#11231 = CARTESIAN_POINT ( 'NONE',  ( 1.317756351988342622, -3.857995168970215438, -0.04852650426602527628 ) ) ;
#11232 = CARTESIAN_POINT ( 'NONE',  ( 146.0000000000002274, -801.0618695410406644, -29.99999999999356604 ) ) ;
#11233 = COLOUR_RGB ( '',0.8941176470588234615, 0.8941176470588234615, 0.8941176470588234615 ) ;
#11234 = AXIS2_PLACEMENT_3D ( 'NONE', #16507, #5282, #13047 ) ;
#11235 = EDGE_LOOP ( 'NONE', ( #16347, #11390, #1675, #15506, #20604, #21898 ) ) ;
#11236 = CIRCLE ( 'NONE', #13177, 35.00000000000000000 ) ;
#11237 = CARTESIAN_POINT ( 'NONE',  ( 1.500000000000000000, 9.886859966642589370, 200.0000119999999981 ) ) ;
#11238 = CARTESIAN_POINT ( 'NONE',  ( 0.000000000000000000, 2.357898499370434386, -3.469446951953614189E-15 ) ) ;
#11239 = DIRECTION ( 'NONE',  ( 0.000000000000000000, 0.000000000000000000, -1.000000000000000000 ) ) ;
#11240 = EDGE_LOOP ( 'NONE', ( #2641, #22906, #22110, #1767 ) ) ;
#11241 = CARTESIAN_POINT ( 'NONE',  ( -285.2000000000000455, 269.9999999999999432, -146.4928932188134070 ) ) ;
#11242 = LINE ( 'NONE', #5419, #17067 ) ;
#11243 = CARTESIAN_POINT ( 'NONE',  ( -1.308996938995744985, -10.00000000000000000, 200.0000119999999697 ) ) ;
#11244 = EDGE_LOOP ( 'NONE', ( #4657, #17847 ) ) ;
#11245 = ADVANCED_FACE ( 'NONE', ( #1001 ), #19721, .F. ) ;
#11246 = CARTESIAN_POINT ( 'NONE',  ( 0.000000000000000000, 2.357898499370431722, -2.818925648462311528E-15 ) ) ;
#11247 = CARTESIAN_POINT ( 'NONE',  ( -285.2000000000011255, -29.99999999999898037, -105.0000000000000000 ) ) ;
#11248 = CARTESIAN_POINT ( 'NONE',  ( 124.2727838502222966, -1092.635313011623566, -27.51610016701187789 ) ) ;
#11249 = ADVANCED_FACE ( 'NONE', ( #19594 ), #19470, .F. ) ;
#11250 = CARTESIAN_POINT ( 'NONE',  ( -6.259644161404860030E-16, -4.618802153517027165, -3.433295621305388234 ) ) ;
#11251 = ORIENTED_EDGE ( 'NONE', *, *, #5173, .T. ) ;
#11252 = CYLINDRICAL_SURFACE ( 'NONE', #13574, 8.000000000000000000 ) ;
#11253 = APPLICATION_PROTOCOL_DEFINITION ( 'draft international standard', 'automotive_design', 1998, #7866 ) ;
#11254 = FACE_BOUND ( 'NONE', #5305, .T. ) ;
#11255 = EDGE_CURVE ( 'NONE', #7372, #13225, #17920, .T. ) ;
#11256 = CARTESIAN_POINT ( 'NONE',  ( -6.486836893983275232, 4.915077010913945443, -7.231838333420560261 ) ) ;
#11257 = CARTESIAN_POINT ( 'NONE',  ( 0.6666666666666689611, 4.233901974057261874, -3.300726591567082480 ) ) ;
#11258 = EDGE_CURVE ( 'NONE', #20911, #23190, #16554, .T. ) ;
#11259 = ORIENTED_EDGE ( 'NONE', *, *, #9883, .F. ) ;
#11260 = ORIENTED_EDGE ( 'NONE', *, *, #12126, .T. ) ;
#11261 = CARTESIAN_POINT ( 'NONE',  ( 0.000000000000000000, -2.357898499370432610, 3.252606517456513302E-15 ) ) ;
#11262 = ADVANCED_FACE ( 'NONE', ( #15758 ), #5729, .F. ) ;
#11263 = EDGE_CURVE ( 'NONE', #436, #1277, #21416, .T. ) ;
#11264 = VERTEX_POINT ( 'NONE', #11145 ) ;
#11265 = DIRECTION ( 'NONE',  ( -1.000000000000000000, -0.000000000000000000, -0.000000000000000000 ) ) ;
#11266 = CARTESIAN_POINT ( 'NONE',  ( 281.4928932188134354, -127.0000000000000568, -152.4000000000012847 ) ) ;
#11267 = ORIENTED_EDGE ( 'NONE', *, *, #22085, .T. ) ;
#11268 = CARTESIAN_POINT ( 'NONE',  ( -137.5000000000000000, -5.062647941322544249E-13, -90.00000000000000000 ) ) ;
#11269 = VERTEX_POINT ( 'NONE', #1801 ) ;
#11270 = DIRECTION ( 'NONE',  ( 0.000000000000000000, 0.000000000000000000, 1.000000000000000000 ) ) ;
#11271 = CARTESIAN_POINT ( 'NONE',  ( 281.4928932188134354, -129.2000000000000455, -177.2000000000013529 ) ) ;
#11272 = VERTEX_POINT ( 'NONE', #23223 ) ;
#11273 = CARTESIAN_POINT ( 'NONE',  ( -7.922281120364393914, -4.573931137438277617, -8.047472243342932430 ) ) ;
#11274 = DIRECTION ( 'NONE',  ( 1.000000000000000000, -3.495664435217746987E-15, -0.000000000000000000 ) ) ;
#11275 = EDGE_CURVE ( 'NONE', #8989, #4643, #14472, .T. ) ;
#11276 = SURFACE_SIDE_STYLE ('',( #18352 ) ) ;
#11277 = EDGE_CURVE ( 'NONE', #2262, #20612, #4755, .T. ) ;
#11278 = LINE ( 'NONE', #18587, #5718 ) ;
#11279 = CARTESIAN_POINT ( 'NONE',  ( 125.5963796794996341, -1090.832610870657163, -31.65735141704666233 ) ) ;
#11280 = CARTESIAN_POINT ( 'NONE',  ( 0.000000000000000000, 0.000000000000000000, 0.000000000000000000 ) ) ;
#11281 = VERTEX_POINT ( 'NONE', #14085 ) ;
#11282 = EDGE_CURVE ( 'NONE', #11372, #19431, #14752, .T. ) ;
#11283 = LINE ( 'NONE', #6041, #10327 ) ;
#11284 = DIRECTION ( 'NONE',  ( -0.000000000000000000, 1.000000000000000000, -3.469446951953613794E-15 ) ) ;
#11285 = PRESENTATION_STYLE_ASSIGNMENT (( #9084 ) ) ;
#11287 = ORIENTED_EDGE ( 'NONE', *, *, #13790, .F. ) ;
#11286 = ORIENTED_EDGE ( 'NONE', *, *, #15952, .F. ) ;
#11288 = EDGE_CURVE ( 'NONE', #13791, #12343, #12285, .T. ) ;
#11289 = DIRECTION ( 'NONE',  ( 1.000000000000000000, 6.123233995736766036E-17, -6.123233995736764803E-17 ) ) ;
#11290 = CARTESIAN_POINT ( 'NONE',  ( 93.00000000000000000, -149.9999999999996874, 129.9038105676659711 ) ) ;
#11291 = CARTESIAN_POINT ( 'NONE',  ( -35.00000000000001421, 90.00000000000001421, 0.000000000000000000 ) ) ;
#11292 = EDGE_CURVE ( 'NONE', #931, #2917, #5556, .T. ) ;
#11293 = VERTEX_POINT ( 'NONE', #14201 ) ;
#11294 = DIRECTION ( 'NONE',  ( -3.469446951953614682E-16, 1.000000000000000000, -3.483493295888648978E-15 ) ) ;
#11295 = EDGE_LOOP ( 'NONE', ( #23602, #10842, #7625, #20386 ) ) ;
#11296 = DIRECTION ( 'NONE',  ( 1.000000000000000000, 0.000000000000000000, 0.000000000000000000 ) ) ;
#11297 = ORIENTED_EDGE ( 'NONE', *, *, #22293, .T. ) ;
#11298 = FACE_OUTER_BOUND ( 'NONE', #16364, .T. ) ;
#11299 = CARTESIAN_POINT ( 'NONE',  ( 99.99999999999997158, 34.99999999999995026, 147.2000000000010971 ) ) ;
#11300 = ITEM_DEFINED_TRANSFORMATION ( 'NONE', 'NONE', #15850,  #11210 ) ;
#11301 = EDGE_LOOP ( 'NONE', ( #5024, #3714, #15495, #4061, #6152, #15042 ) ) ;
#11302 = DIRECTION ( 'NONE',  ( -1.000000000000000000, 0.000000000000000000, 0.000000000000000000 ) ) ;
#11303 = VERTEX_POINT ( 'NONE', #21535 ) ;
#11304 = FACE_OUTER_BOUND ( 'NONE', #3335, .T. ) ;
#11305 = CARTESIAN_POINT ( 'NONE',  ( -0.3461262719736137305, 4.658553426539289610, -3.671615880910373608 ) ) ;
#11306 = AXIS2_PLACEMENT_3D ( 'NONE', #16404, #99, #14841 ) ;
#11307 = CARTESIAN_POINT ( 'NONE',  ( 1.747541505913279281, -3.837784562140273081, -3.503702292528912299 ) ) ;
#11308 = CARTESIAN_POINT ( 'NONE',  ( 72.64999999999999147, -87.33333333333332860, 124.9999999999999858 ) ) ;
#11309 = CARTESIAN_POINT ( 'NONE',  ( -281.4533442688713762, 269.4578961534456312, 145.6839617489740988 ) ) ;
#11310 = ORIENTED_EDGE ( 'NONE', *, *, #3276, .T. ) ;
#11311 = CARTESIAN_POINT ( 'NONE',  ( 0.000000000000000000, 0.000000000000000000, 0.000000000000000000 ) ) ;
#11312 = EDGE_CURVE ( 'NONE', #748, #1893, #10579, .T. ) ;
#11313 = DIRECTION ( 'NONE',  ( 0.000000000000000000, 0.000000000000000000, 1.000000000000000000 ) ) ;
#11314 = CARTESIAN_POINT ( 'NONE',  ( 50.00000000000000000, 0.000000000000000000, 4.171999999999999709 ) ) ;
#11315 = EDGE_CURVE ( 'NONE', #16783, #4691, #20608, .T. ) ;
#11316 = EDGE_CURVE ( 'NONE', #9249, #2180, #13440, .T. ) ;
#11317 = DIRECTION ( 'NONE',  ( -1.000000000000000000, -2.775557561562891351E-17, 0.000000000000000000 ) ) ;
#11318 = LINE ( 'NONE', #5848, #9114 ) ;
#11319 = TOROIDAL_SURFACE ( 'NONE', #20918, 4.000000000000000000, 0.2500000000000000000 ) ;
#11320 = CYLINDRICAL_SURFACE ( 'NONE', #11781, 2.500000000000002220 ) ;
#11321 = DIRECTION ( 'NONE',  ( -0.000000000000000000, -0.000000000000000000, 1.000000000000000000 ) ) ;
#11322 = ITEM_DEFINED_TRANSFORMATION ( 'NONE', 'NONE', #8101,  #11210 ) ;
#11323 = ORIENTED_EDGE ( 'NONE', *, *, #15028, .F. ) ;
#11324 = CARTESIAN_POINT ( 'NONE',  ( -24.99999999999998224, -998.3637538262555609, 145.0000119999999697 ) ) ;
#11325 = ORIENTED_EDGE ( 'NONE', *, *, #18716, .F. ) ;
#11326 = FACE_OUTER_BOUND ( 'NONE', #14890, .T. ) ;
#11327 = CARTESIAN_POINT ( 'NONE',  ( -280.0000000000000568, 272.9999999999999432, 145.0000000000000284 ) ) ;
#11328 = ORIENTED_EDGE ( 'NONE', *, *, #20821, .T. ) ;
#11329 = DIRECTION ( 'NONE',  ( 0.000000000000000000, 0.000000000000000000, 1.000000000000000000 ) ) ;
#11330 = CARTESIAN_POINT ( 'NONE',  ( 2.500000000000000000, 0.000000000000000000, 0.000000000000000000 ) ) ;
#11331 = FACE_OUTER_BOUND ( 'NONE', #10270, .T. ) ;
#11332 = DIRECTION ( 'NONE',  ( -0.5000000000000051070, 1.060575238724903217E-16, -0.8660254037844355990 ) ) ;
#11333 = DIRECTION ( 'NONE',  ( 0.000000000000000000, 0.000000000000000000, -1.000000000000000000 ) ) ;
#11334 = DIRECTION ( 'NONE',  ( 0.000000000000000000, 0.000000000000000000, 1.000000000000000000 ) ) ;
#11335 = CARTESIAN_POINT ( 'NONE',  ( -23.72315261474503600, 8.055391459054607850, 145.0000119999999697 ) ) ;
#11336 = AXIS2_PLACEMENT_3D ( 'NONE', #21700, #5158, #10873 ) ;
#11337 = ORIENTED_EDGE ( 'NONE', *, *, #19808, .F. ) ;
#11338 = CARTESIAN_POINT ( 'NONE',  ( 0.000000000000000000, 0.000000000000000000, -10.00000000000000000 ) ) ;
#11339 = DIRECTION ( 'NONE',  ( 0.000000000000000000, 2.838638415234739015E-14, -1.000000000000000000 ) ) ;
#11340 = EDGE_LOOP ( 'NONE', ( #19582, #1475, #15188, #7156 ) ) ;
#11341 = EDGE_CURVE ( 'NONE', #19646, #19464, #10172, .T. ) ;
#11342 = CARTESIAN_POINT ( 'NONE',  ( -110.0000000000000000, -94.99999999999997158, 3.000000000000000000 ) ) ;
#11343 = LINE ( 'NONE', #9876, #17666 ) ;
#11344 = PLANE ( 'NONE',  #12193 ) ;
#11345 = PRESENTATION_LAYER_ASSIGNMENT (  '', '', ( #6700 ) ) ;
#11346 = ORIENTED_EDGE ( 'NONE', *, *, #3802, .T. ) ;
#11347 = DIRECTION ( 'NONE',  ( 0.000000000000000000, 0.000000000000000000, 1.000000000000000000 ) ) ;
#11348 = CARTESIAN_POINT ( 'NONE',  ( -4.000000000000000000, 2.309401076758498483, -0.4999999999999927280 ) ) ;
#11349 = DIRECTION ( 'NONE',  ( 0.000000000000000000, 0.4999999999999991118, -0.8660254037844390407 ) ) ;
#11350 = ORIENTED_EDGE ( 'NONE', *, *, #20075, .T. ) ;
#11351 = DIRECTION ( 'NONE',  ( -1.000000000000000000, -0.000000000000000000, -0.000000000000000000 ) ) ;
#11352 = DIRECTION ( 'NONE',  ( 0.000000000000000000, -0.000000000000000000, 1.000000000000000000 ) ) ;
#11353 = CARTESIAN_POINT ( 'NONE',  ( -1.240299975428134203E-15, -4.736529461165891242, -3.681130640444276292 ) ) ;
#11354 = ORIENTED_EDGE ( 'NONE', *, *, #12630, .F. ) ;
#11355 = DIRECTION ( 'NONE',  ( 0.000000000000000000, 1.000000000000000000, 0.000000000000000000 ) ) ;
#11356 = SHAPE_DEFINITION_REPRESENTATION ( #8435, #22995 ) ;
#11357 = CARTESIAN_POINT ( 'NONE',  ( 7.922281120364393914, 4.573931137438269623, -8.047472243342930653 ) ) ;
#11358 = CARTESIAN_POINT ( 'NONE',  ( 52.00000000000000711, 0.000000000000000000, 0.000000000000000000 ) ) ;
#11359 = DIRECTION ( 'NONE',  ( 0.000000000000000000, 0.000000000000000000, 1.000000000000000000 ) ) ;
#11360 = VECTOR ( 'NONE', #5424, 1000.000000000000114 ) ;
#11361 = ORIENTED_EDGE ( 'NONE', *, *, #5192, .F. ) ;
#11362 = VECTOR ( 'NONE', #18640, 1000.000000000000000 ) ;
#11363 = VERTEX_POINT ( 'NONE', #18813 ) ;
#11364 = DIRECTION ( 'NONE',  ( -0.9423651898111408132, -0.3345860861306287348, 6.982962677686266711E-15 ) ) ;
#11365 = LINE ( 'NONE', #22435, #4454 ) ;
#11366 = EDGE_CURVE ( 'NONE', #12940, #9524, #14992, .T. ) ;
#11367 = EDGE_CURVE ( 'NONE', #4420, #16878, #11396, .T. ) ;
#11368 = ADVANCED_FACE ( 'NONE', ( #20632 ), #22332, .F. ) ;
#11369 = ORIENTED_EDGE ( 'NONE', *, *, #8740, .F. ) ;
#11370 = CYLINDRICAL_SURFACE ( 'NONE', #8277, 2.649999999999985700 ) ;
#11371 = DIRECTION ( 'NONE',  ( 0.000000000000000000, 0.000000000000000000, -1.000000000000000000 ) ) ;
#11372 = VERTEX_POINT ( 'NONE', #1930 ) ;
#11373 = FACE_OUTER_BOUND ( 'NONE', #839, .T. ) ;
#11374 = ADVANCED_FACE ( 'NONE', ( #13214 ), #13319, .F. ) ;
#11375 = AXIS2_PLACEMENT_3D ( 'NONE', #6132, #17587, #922 ) ;
#11376 = ORIENTED_EDGE ( 'NONE', *, *, #19779, .T. ) ;
#11377 = CIRCLE ( 'NONE', #4803, 20.00000000000000000 ) ;
#11378 = DIRECTION ( 'NONE',  ( -1.000000000000000000, -0.000000000000000000, -0.000000000000000000 ) ) ;
#11379 = CARTESIAN_POINT ( 'NONE',  ( -122.8605704798721945, 82.74225173005939382, -29.99999999999356604 ) ) ;
#11380 = ORIENTED_EDGE ( 'NONE', *, *, #1775, .F. ) ;
#11381 = ORIENTED_EDGE ( 'NONE', *, *, #613, .F. ) ;
#11382 = CARTESIAN_POINT ( 'NONE',  ( -128.9689330775208020, 85.97690438148627834, -31.65735141704659128 ) ) ;
#11383 = ADVANCED_FACE ( 'NONE', ( #6030 ), #11639, .T. ) ;
#11384 = CARTESIAN_POINT ( 'NONE',  ( -280.1245861693740267, 272.9663417894422537, -145.6816199723480452 ) ) ;
#11385 = CARTESIAN_POINT ( 'NONE',  ( -23.72315261474500758, -1008.055391459054704, 145.0000119999999697 ) ) ;
#11386 = LINE ( 'NONE', #22571, #704 ) ;
#11387 = CARTESIAN_POINT ( 'NONE',  ( -112.7436279071525433, -91.18044947428992941, -2.775557561562891351E-14 ) ) ;
#11388 = DIRECTION ( 'NONE',  ( 0.000000000000000000, 0.000000000000000000, 1.000000000000000000 ) ) ;
#11389 = CARTESIAN_POINT ( 'NONE',  ( 132.8404720734530144, 79.86494211668949106, 27.50000000000646239 ) ) ;
#11390 = ORIENTED_EDGE ( 'NONE', *, *, #15368, .F. ) ;
#11391 = CIRCLE ( 'NONE', #178, 2.055000000000001492 ) ;
#11392 = DIRECTION ( 'NONE',  ( 0.000000000000000000, 0.000000000000000000, 1.000000000000000000 ) ) ;
#11393 = CARTESIAN_POINT ( 'NONE',  ( -146.4450000000005048, -494.4690652294800088, -27.49999999999356604 ) ) ;
#11395 = ORIENTED_EDGE ( 'NONE', *, *, #14063, .F. ) ;
#11394 = EDGE_LOOP ( 'NONE', ( #8991, #16420, #17074, #15796 ) ) ;
#11396 = CIRCLE ( 'NONE', #23696, 2.649999999999999467 ) ;
#11397 = CARTESIAN_POINT ( 'NONE',  ( 91.18044947429038416, -112.7436279071521881, -2.775557561562891351E-14 ) ) ;
#11398 = DIRECTION ( 'NONE',  ( 1.000000000000000000, -0.000000000000000000, 6.982962677686266711E-15 ) ) ;
#11399 = EDGE_LOOP ( 'NONE', ( #15061, #21786 ) ) ;
#11400 = CIRCLE ( 'NONE', #9453, 2.499999999999998668 ) ;
#11401 = CARTESIAN_POINT ( 'NONE',  ( -134.5810953439728053, -1076.895678479288563, 29.34395718620174165 ) ) ;
#11402 = ORIENTED_EDGE ( 'NONE', *, *, #16396, .F. ) ;
#11403 = ADVANCED_FACE ( 'NONE', ( #3863 ), #3964, .F. ) ;
#11404 = FACE_OUTER_BOUND ( 'NONE', #22074, .T. ) ;
#11405 = ADVANCED_FACE ( 'NONE', ( #9428 ), #18581, .F. ) ;
#11406 = ORIENTED_EDGE ( 'NONE', *, *, #62, .T. ) ;
#11407 = CONICAL_SURFACE ( 'NONE', #5984, 4.000000000000000000, 0.8911886515913786111 ) ;
#11408 = CARTESIAN_POINT ( 'NONE',  ( -45.00000000000000711, 0.000000000000000000, 169.9999999999999716 ) ) ;
#11409 = FILL_AREA_STYLE_COLOUR ( '', #745 ) ;
#11410 = ORIENTED_EDGE ( 'NONE', *, *, #4096, .T. ) ;
#11411 =( REPRESENTATION_RELATIONSHIP ('NONE','NONE', #10127, #4815 ) REPRESENTATION_RELATIONSHIP_WITH_TRANSFORMATION ( #4737 )SHAPE_REPRESENTATION_RELATIONSHIP( ) );
#11412 = EDGE_CURVE ( 'NONE', #12624, #3444, #22489, .T. ) ;
#11413 = AXIS2_PLACEMENT_3D ( 'NONE', #485, #2148, #9540 ) ;
#11414 = PRODUCT_RELATED_PRODUCT_CATEGORY ( 'part', '', ( #17885 ) ) ;
#11415 = FACE_BOUND ( 'NONE', #6632, .T. ) ;
#11416 = VERTEX_POINT ( 'NONE', #605 ) ;
#11417 = EDGE_CURVE ( 'NONE', #10051, #3871, #7969, .T. ) ;
#11418 = CARTESIAN_POINT ( 'NONE',  ( -128.6132171834567544, 86.50814704276137945, 27.82811892742373416 ) ) ;
#11419 = LINE ( 'NONE', #1965, #20027 ) ;
#11420 = AXIS2_PLACEMENT_3D ( 'NONE', #7543, #1309, #13028 ) ;
#11421 = FACE_BOUND ( 'NONE', #2385, .T. ) ;
#11422 = FACE_OUTER_BOUND ( 'NONE', #23344, .T. ) ;
#11423 = ORIENTED_EDGE ( 'NONE', *, *, #14505, .F. ) ;
#11424 = CARTESIAN_POINT ( 'NONE',  ( -280.2488155364688964, 269.9132285165672442, -145.5679143846942907 ) ) ;
#11425 = PRESENTATION_STYLE_ASSIGNMENT (( #4009 ) ) ;
#11426 = ORIENTED_EDGE ( 'NONE', *, *, #15938, .F. ) ;
#11427 = DIRECTION ( 'NONE',  ( 6.982962677686266711E-15, 0.000000000000000000, -1.000000000000000000 ) ) ;
#11428 = CARTESIAN_POINT ( 'NONE',  ( -281.4928932188134922, -127.0000000000000568, 150.2000000000013813 ) ) ;
#11429 = CARTESIAN_POINT ( 'NONE',  ( 235.0000000000000284, -500.0000000000001137, -59.99999999999997868 ) ) ;
#11430 = CARTESIAN_POINT ( 'NONE',  ( 281.3333820183295302, 269.5350371479512432, 145.6220388411722695 ) ) ;
#11431 = DIRECTION ( 'NONE',  ( 0.000000000000000000, 0.000000000000000000, 1.000000000000000000 ) ) ;
#11432 = CIRCLE ( 'NONE', #11054, 2.649999999999971934 ) ;
#11433 = DIRECTION ( 'NONE',  ( 1.000000000000000000, 0.000000000000000000, 0.000000000000000000 ) ) ;
#11434 = CARTESIAN_POINT ( 'NONE',  ( 123.7129353098591480, -1093.381627813013665, 32.17229779615543350 ) ) ;
#11435 = ORIENTED_EDGE ( 'NONE', *, *, #15826, .F. ) ;
#11436 = CARTESIAN_POINT ( 'NONE',  ( -22.47082401081930314, -988.9212198408002905, 145.0000119999999697 ) ) ;
#11437 = VERTEX_POINT ( 'NONE', #22449 ) ;
#11438 = LINE ( 'NONE', #2098, #9880 ) ;
#11439 = DIRECTION ( 'NONE',  ( 0.000000000000000000, 1.000000000000000000, 0.000000000000000000 ) ) ;
#11440 = EDGE_CURVE ( 'NONE', #7122, #21239, #5908, .T. ) ;
#11441 = EDGE_CURVE ( 'NONE', #14374, #5614, #7463, .T. ) ;
#11442 = AXIS2_PLACEMENT_3D ( 'NONE', #16144, #3667, #12559 ) ;
#11443 = EDGE_CURVE ( 'NONE', #949, #10543, #14054, .T. ) ;
#11444 = CARTESIAN_POINT ( 'NONE',  ( -285.2000000000008981, 35.00000000000100897, 105.0000000000000000 ) ) ;
#11445 = ORIENTED_EDGE ( 'NONE', *, *, #14744, .T. ) ;
#11446 = CYLINDRICAL_SURFACE ( 'NONE', #15411, 145.0000000000000284 ) ;
#11447 = FACE_BOUND ( 'NONE', #2629, .T. ) ;
#11448 = CARTESIAN_POINT ( 'NONE',  ( 0.000000000000000000, 0.000000000000000000, 0.000000000000000000 ) ) ;
#11449 = CARTESIAN_POINT ( 'NONE',  ( -40.00000000000000000, 100.0000000000000000, -147.2000000000005571 ) ) ;
#11450 = DIRECTION ( 'NONE',  ( -0.5877852522924773560, 0.8090169943749444537, 0.000000000000000000 ) ) ;
#11451 = DIRECTION ( 'NONE',  ( -1.000000000000000000, -3.202566417187951028E-16, -6.405132834375902056E-16 ) ) ;
#11452 = CARTESIAN_POINT ( 'NONE',  ( -7.897827455343210623, -1.533134349199909208, -7.633632140068262295 ) ) ;
#11453 = VERTEX_POINT ( 'NONE', #22686 ) ;
#11454 =( NAMED_UNIT ( * ) PLANE_ANGLE_UNIT ( ) SI_UNIT ( $, .RADIAN. ) );
#11455 = PLANE ( 'NONE',  #21890 ) ;
#11456 = DIRECTION ( 'NONE',  ( 0.000000000000000000, 0.000000000000000000, -1.000000000000000000 ) ) ;
#11457 = ORIENTED_EDGE ( 'NONE', *, *, #19119, .F. ) ;
#11458 = VERTEX_POINT ( 'NONE', #6159 ) ;
#11459 = CARTESIAN_POINT ( 'NONE',  ( 281.4928932188133217, -127.0000000000000568, 152.4000000000014268 ) ) ;
#11460 = DIRECTION ( 'NONE',  ( -1.000000000000000000, -0.000000000000000000, -0.000000000000000000 ) ) ;
#11461 = AXIS2_PLACEMENT_3D ( 'NONE', #6682, #9963, #17660 ) ;
#11462 = CARTESIAN_POINT ( 'NONE',  ( 281.4928932188133786, 269.9999999999999432, 147.1999999999999886 ) ) ;
#11463 = ORIENTED_EDGE ( 'NONE', *, *, #2348, .F. ) ;
#11464 = CIRCLE ( 'NONE', #2159, 7.500000000000004441 ) ;
#11465 = PLANE ( 'NONE',  #19971 ) ;
#11466 = CARTESIAN_POINT ( 'NONE',  ( 0.000000000000000000, 0.000000000000000000, -90.00000000000000000 ) ) ;
#11467 = CARTESIAN_POINT ( 'NONE',  ( 2.617478843592798921, -9.739726766683157066, 200.0000119999999981 ) ) ;
#11468 = ORIENTED_EDGE ( 'NONE', *, *, #8719, .F. ) ;
#11469 = DIRECTION ( 'NONE',  ( 1.000000000000000000, 0.000000000000000000, 0.000000000000000000 ) ) ;
#11470 = CARTESIAN_POINT ( 'NONE',  ( 44.80746418436557832, 137.9031948627978750, 90.00000000000000000 ) ) ;
#11471 = ORIENTED_EDGE ( 'NONE', *, *, #23610, .F. ) ;
#11472 = VECTOR ( 'NONE', #1813, 1000.000000000000000 ) ;
#11473 = CARTESIAN_POINT ( 'NONE',  ( 285.1999999999999318, 267.7999999999999545, -146.4928932188133786 ) ) ;
#11474 = SHAPE_REPRESENTATION ( 'socket head cap screw_iso_ISO 4762 M10 x 40 - 40N', ( #11210 ), #21934 ) ;
#11475 = PRODUCT_DEFINITION_SHAPE ( 'NONE', 'NONE',  #23888 ) ;
#11476 = PRODUCT_CONTEXT ( 'NONE', #4898, 'mechanical' ) ;
#11477 = CARTESIAN_POINT ( 'NONE',  ( 37.64999999999996305, 90.00000000000000000, 0.000000000000000000 ) ) ;
#11478 = VECTOR ( 'NONE', #10691, 1000.000000000000114 ) ;
#11479 = CARTESIAN_POINT ( 'NONE',  ( -7.112481253775184697, 4.553861071372892866, -7.781689322728085223 ) ) ;
#11480 = DIRECTION ( 'NONE',  ( -1.000000000000000000, 0.000000000000000000, 0.000000000000000000 ) ) ;
#11481 = ORIENTED_EDGE ( 'NONE', *, *, #157, .F. ) ;
#11482 = EDGE_LOOP ( 'NONE', ( #23267, #4564 ) ) ;
#11483 = FACE_OUTER_BOUND ( 'NONE', #607, .T. ) ;
#11484 = DIRECTION ( 'NONE',  ( 0.000000000000000000, 0.000000000000000000, -1.000000000000000000 ) ) ;
#11485 = PRODUCT_DEFINITION_CONTEXT ( 'detailed design', #13123, 'design' ) ;
#11486 = AXIS2_PLACEMENT_3D ( 'NONE', #13675, #20995, #2141 ) ;
#11487 = VERTEX_POINT ( 'NONE', #18472 ) ;
#11488 = DIRECTION ( 'NONE',  ( -1.000000000000000000, -0.000000000000000000, -0.000000000000000000 ) ) ;
#11489 = DIRECTION ( 'NONE',  ( 6.982962677686266711E-15, -9.837870180509810443E-29, 1.000000000000000000 ) ) ;
#11490 = ORIENTED_EDGE ( 'NONE', *, *, #4589, .F. ) ;
#11491 = VECTOR ( 'NONE', #16544, 1000.000000000000114 ) ;
#11492 = DIRECTION ( 'NONE',  ( 0.000000000000000000, -0.4999999999999987788, 0.8660254037844392627 ) ) ;
#11493 = VECTOR ( 'NONE', #13056, 1000.000000000000000 ) ;
#11494 = ADVANCED_FACE ( 'NONE', ( #13085 ), #12134, .T. ) ;
#11495 = EDGE_LOOP ( 'NONE', ( #15192, #17731, #14327, #12492 ) ) ;
#11496 = CARTESIAN_POINT ( 'NONE',  ( 0.000000000000000000, 0.000000000000000000, 200.0000119999999981 ) ) ;
#11497 = DIRECTION ( 'NONE',  ( 1.000000000000000000, 0.000000000000000000, 0.000000000000000000 ) ) ;
#11498 = ORIENTED_EDGE ( 'NONE', *, *, #16241, .T. ) ;
#11499 = ORIENTED_EDGE ( 'NONE', *, *, #19348, .T. ) ;
#11500 = DIRECTION ( 'NONE',  ( 1.110223024625157172E-14, 0.000000000000000000, -1.000000000000000000 ) ) ;
#11501 = ADVANCED_FACE ( 'NONE', ( #2767, #8217 ), #2526, .T. ) ;
#11502 = LINE ( 'NONE', #4225, #7720 ) ;
#11503 = LINE ( 'NONE', #2965, #3605 ) ;
#11504 = ADVANCED_FACE ( 'NONE', ( #21360 ), #8105, .F. ) ;
#11505 = AXIS2_PLACEMENT_3D ( 'NONE', #701, #17258, #11738 ) ;
#11506 = DIRECTION ( 'NONE',  ( 0.000000000000000000, 0.000000000000000000, -1.000000000000000000 ) ) ;
#11507 = CARTESIAN_POINT ( 'NONE',  ( -90.00000000000000000, 3.053113317719180486E-13, 129.9038105676659711 ) ) ;
#11508 = CARTESIAN_POINT ( 'NONE',  ( 279.9999999999999432, 273.0000000000000000, -144.9999999999999716 ) ) ;
#11509 = DIRECTION ( 'NONE',  ( -3.495664435217746987E-15, 1.000000000000000000, 0.000000000000000000 ) ) ;
#11510 = EDGE_LOOP ( 'NONE', ( #1222, #1970, #6387, #12828 ) ) ;
#11511 = FACE_BOUND ( 'NONE', #17339, .T. ) ;
#11512 = AXIS2_PLACEMENT_3D ( 'NONE', #4280, #18992, #5965 ) ;
#11513 = DIRECTION ( 'NONE',  ( -0.000000000000000000, -0.000000000000000000, 1.000000000000000000 ) ) ;
#11514 = EDGE_CURVE ( 'NONE', #17056, #10547, #2644, .T. ) ;
#11515 = AXIS2_PLACEMENT_3D ( 'NONE', #15245, #5925, #18592 ) ;
#11516 = CIRCLE ( 'NONE', #23037, 2.649999999999971934 ) ;
#11517 = ORIENTED_EDGE ( 'NONE', *, *, #15916, .T. ) ;
#11518 = CARTESIAN_POINT ( 'NONE',  ( 7.499999999999997335, 34.18698582794336005, -100.0000000000000000 ) ) ;
#11519 = CARTESIAN_POINT ( 'NONE',  ( 279.9999999999999432, 273.0299999999999727, -144.9999999999999716 ) ) ;
#11520 = EDGE_LOOP ( 'NONE', ( #956, #9390, #17150, #13613 ) ) ;
#11521 = CARTESIAN_POINT ( 'NONE',  ( -134.7167544493337914, -1076.657711551589728, 31.26048023074365290 ) ) ;
#11522 = ORIENTED_EDGE ( 'NONE', *, *, #15278, .T. ) ;
#11523 = CIRCLE ( 'NONE', #307, 5.000000000000000888 ) ;
#11524 = DIRECTION ( 'NONE',  ( 1.350636282998972974E-14, 0.000000000000000000, -1.000000000000000000 ) ) ;
#11525 = ORIENTED_EDGE ( 'NONE', *, *, #18781, .F. ) ;
#11526 = CARTESIAN_POINT ( 'NONE',  ( 2.500000000000000000, 2.357898499370431722, -2.818925648462311528E-15 ) ) ;
#11527 = VECTOR ( 'NONE', #1852, 1000.000000000000000 ) ;
#11528 =( NAMED_UNIT ( * ) PLANE_ANGLE_UNIT ( ) SI_UNIT ( $, .RADIAN. ) );
#11529 = AXIS2_PLACEMENT_3D ( 'NONE', #21338, #17717, #1174 ) ;
#11530 = ORIENTED_EDGE ( 'NONE', *, *, #13697, .F. ) ;
#11531 = VECTOR ( 'NONE', #8059, 1000.000000000000000 ) ;
#11532 = CYLINDRICAL_SURFACE ( 'NONE', #15287, 35.00000000000000711 ) ;
#11533 = ORIENTED_EDGE ( 'NONE', *, *, #12332, .T. ) ;
#11534 = CARTESIAN_POINT ( 'NONE',  ( 1.642023387942651569, -974.9999507392942633, -145.0000000000001137 ) ) ;
#11535 = LINE ( 'NONE', #15267, #4604 ) ;
#11536 = DIRECTION ( 'NONE',  ( -1.350636282998972974E-14, 0.000000000000000000, -1.000000000000000000 ) ) ;
#11537 = CARTESIAN_POINT ( 'NONE',  ( -100.0000000000001137, -129.2000000000000455, 177.2000000000014097 ) ) ;
#11538 = ORIENTED_EDGE ( 'NONE', *, *, #12300, .F. ) ;
#11539 = CARTESIAN_POINT ( 'NONE',  ( -280.0000000000000568, 269.9999999999999432, 145.0000000000000284 ) ) ;
#11540 =( LENGTH_UNIT ( ) NAMED_UNIT ( * ) SI_UNIT ( .MILLI., .METRE. ) );
#11541 = EDGE_CURVE ( 'NONE', #20119, #10574, #15706, .T. ) ;
#11542 = ADVANCED_FACE ( 'NONE', ( #21481, #23042 ), #8573, .T. ) ;
#11544 = ORIENTED_EDGE ( 'NONE', *, *, #13943, .T. ) ;
#11543 = ORIENTED_EDGE ( 'NONE', *, *, #23711, .T. ) ;
#11545 = VECTOR ( 'NONE', #18405, 1000.000000000000000 ) ;
#11546 = CARTESIAN_POINT ( 'NONE',  ( -163.0000000000000853, -204.4690652294804920, 30.00000000000653699 ) ) ;
#11547 = AXIS2_PLACEMENT_3D ( 'NONE', #19008, #8045, #4299 ) ;
#11548 = DIRECTION ( 'NONE',  ( 0.4924295582441687857, -0.5074575156280874966, 0.7071067811865630048 ) ) ;
#11549 = DIRECTION ( 'NONE',  ( -0.8090169943749507819, 0.5877852522924686962, 0.000000000000000000 ) ) ;
#11550 = CIRCLE ( 'NONE', #9989, 2.649999999999971934 ) ;
#11551 = AXIS2_PLACEMENT_3D ( 'NONE', #22212, #11156, #7608 ) ;
#11552 = ADVANCED_FACE ( 'NONE', ( #15594, #22921, #13687 ), #2870, .T. ) ;
#11553 = CARTESIAN_POINT ( 'NONE',  ( 281.7350371479512319, 269.1333820183295416, 145.8708543776412228 ) ) ;
#11554 = DIRECTION ( 'NONE',  ( 1.000000000000000000, 0.000000000000000000, 0.000000000000000000 ) ) ;
#11555 = PRODUCT_DEFINITION ( 'UNKNOWN', '', #19665, #2271 ) ;
#11556 = ORIENTED_EDGE ( 'NONE', *, *, #5291, .T. ) ;
#11557 = EDGE_CURVE ( 'NONE', #7464, #3094, #21006, .T. ) ;
#11558 = VECTOR ( 'NONE', #17244, 1000.000000000000000 ) ;
#11559 = CARTESIAN_POINT ( 'NONE',  ( 3.000000000000002665, 0.000000000000000000, 0.000000000000000000 ) ) ;
#11560 = PLANE ( 'NONE',  #14847 ) ;
#11561 = DIRECTION ( 'NONE',  ( 0.000000000000000000, 0.000000000000000000, -1.000000000000000000 ) ) ;
#11562 = ITEM_DEFINED_TRANSFORMATION ( 'NONE', 'NONE', #21596,  #11210 ) ;
#11563 = ORIENTED_EDGE ( 'NONE', *, *, #21180, .T. ) ;
#11564 = CARTESIAN_POINT ( 'NONE',  ( 279.9999999999999432, -127.0000000000000568, 147.2000000000013813 ) ) ;
#11565 = ORIENTED_EDGE ( 'NONE', *, *, #4107, .F. ) ;
#11566 = DIRECTION ( 'NONE',  ( 0.000000000000000000, -0.000000000000000000, -1.000000000000000000 ) ) ;
#11567 = DIRECTION ( 'NONE',  ( 0.000000000000000000, -1.000000000000000000, 0.000000000000000000 ) ) ;
#11569 = CIRCLE ( 'NONE', #4201, 0.2500000000000002220 ) ;
#11568 =( GEOMETRIC_REPRESENTATION_CONTEXT ( 3 ) GLOBAL_UNCERTAINTY_ASSIGNED_CONTEXT ( ( #14745 ) ) GLOBAL_UNIT_ASSIGNED_CONTEXT ( ( #20585, #7011, #8955 ) ) REPRESENTATION_CONTEXT ( 'NONE', 'WORKASPACE' ) );
#11570 = ORIENTED_EDGE ( 'NONE', *, *, #14228, .F. ) ;
#11571 = AXIS2_PLACEMENT_3D ( 'NONE', #8790, #12458, #3674 ) ;
#11572 = DIRECTION ( 'NONE',  ( 0.000000000000000000, -1.000000000000000000, 0.000000000000000000 ) ) ;
#11573 = VECTOR ( 'NONE', #6262, 1000.000000000000000 ) ;
#11574 = EDGE_LOOP ( 'NONE', ( #23488, #5700, #16586, #7165 ) ) ;
#11575 = FACE_OUTER_BOUND ( 'NONE', #17087, .T. ) ;
#11576 = VECTOR ( 'NONE', #4369, 1000.000000000000114 ) ;
#11577 = DIRECTION ( 'NONE',  ( 0.000000000000000000, -3.483493295888648978E-15, -1.000000000000000000 ) ) ;
#11578 = DIRECTION ( 'NONE',  ( 0.7071067811865416886, 0.000000000000000000, -0.7071067811865532349 ) ) ;
#11579 = DIRECTION ( 'NONE',  ( -0.000000000000000000, 1.000000000000000000, -3.469446951953613794E-15 ) ) ;
#11580 = ADVANCED_FACE ( 'NONE', ( #11750 ), #23172, .F. ) ;
#11581 = CARTESIAN_POINT ( 'NONE',  ( -117.3074641843669781, -85.22886158240918064, 90.00000000000000000 ) ) ;
#11582 = CARTESIAN_POINT ( 'NONE',  ( 145.9999999999997726, -801.0618695410399823, 32.05500000000641592 ) ) ;
#11583 = CARTESIAN_POINT ( 'NONE',  ( -24.99999999999999645, -2.129009867111508370E-15, 145.0000059999999849 ) ) ;
#11584 = VERTEX_POINT ( 'NONE', #10048 ) ;
#11585 = SURFACE_SIDE_STYLE ('',( #15777 ) ) ;
#11586 = LINE ( 'NONE', #2597, #4136 ) ;
#11587 = DIRECTION ( 'NONE',  ( -0.5114233182937522049, 0.4883095222350258280, -0.7071067811865532349 ) ) ;
#11588 = EDGE_LOOP ( 'NONE', ( #19869, #14356, #1137 ) ) ;
#11589 = ORIENTED_EDGE ( 'NONE', *, *, #5427, .T. ) ;
#11590 = FACE_OUTER_BOUND ( 'NONE', #12019, .T. ) ;
#11591 = CARTESIAN_POINT ( 'NONE',  ( -155.0000000000000284, -494.4690652294806910, 32.50000000000648015 ) ) ;
#11592 = ADVANCED_FACE ( 'NONE', ( #13802 ), #17399, .T. ) ;
#11594 = VECTOR ( 'NONE', #15536, 1000.000000000000000 ) ;
#11593 = AXIS2_PLACEMENT_3D ( 'NONE', #19572, #8857, #16231 ) ;
#11595 = EDGE_CURVE ( 'NONE', #9869, #1268, #20968, .T. ) ;
#11596 = AXIS2_PLACEMENT_3D ( 'NONE', #2828, #22516, #15305 ) ;
#11597 = VECTOR ( 'NONE', #12273, 1000.000000000000000 ) ;
#11598 = CARTESIAN_POINT ( 'NONE',  ( 281.3405375976307141, 269.5502846751311949, -145.6212670861564220 ) ) ;
#11599 = CIRCLE ( 'NONE', #7695, 45.00000000000000711 ) ;
#11600 = VECTOR ( 'NONE', #324, 1000.000000000000000 ) ;
#11601 = ORIENTED_EDGE ( 'NONE', *, *, #1430, .F. ) ;
#11602 = DIRECTION ( 'NONE',  ( 0.000000000000000000, 0.000000000000000000, 1.000000000000000000 ) ) ;
#11603 = DIRECTION ( 'NONE',  ( 1.000000000000000000, 0.000000000000000000, 0.000000000000000000 ) ) ;
#11604 = B_SPLINE_CURVE_WITH_KNOTS ( 'NONE', 3,
 ( #1795, #20154, #21975, #5549, #3601, #11021 ),
 .UNSPECIFIED., .F., .F.,
 ( 4, 2, 4 ),
 ( -5.145455527296316946E-06, 0.0004153350442917303517, 0.0008358155441107569450 ),
 .UNSPECIFIED. ) ;
#11605 = LINE ( 'NONE', #17241, #1500 ) ;
#11606 = EDGE_LOOP ( 'NONE', ( #4807, #1480 ) ) ;
#11607 = DIRECTION ( 'NONE',  ( 1.000000000000000000, 0.000000000000000000, 0.000000000000000000 ) ) ;
#11608 = DIRECTION ( 'NONE',  ( 0.000000000000000000, 0.000000000000000000, 1.000000000000000000 ) ) ;
#11609 = UNCERTAINTY_MEASURE_WITH_UNIT (LENGTH_MEASURE( 1.000000000000000082E-05 ), #3875, 'distance_accuracy_value', 'NONE');
#11610 = LINE ( 'NONE', #9523, #6716 ) ;
#11611 = ORIENTED_EDGE ( 'NONE', *, *, #21631, .T. ) ;
#11612 = CARTESIAN_POINT ( 'NONE',  ( 281.3333820183295302, 269.5350371479512432, -145.6220388411722126 ) ) ;
#11613 = ITEM_DEFINED_TRANSFORMATION ( 'NONE', 'NONE', #4215,  #11210 ) ;
#11614 = FACE_BOUND ( 'NONE', #6858, .T. ) ;
#11616 = MECHANICAL_DESIGN_GEOMETRIC_PRESENTATION_REPRESENTATION (  '', ( #21973 ), #4238 ) ;
#11615 = PRODUCT_DEFINITION_FORMATION_WITH_SPECIFIED_SOURCE ( 'ANY', '', #10385, .NOT_KNOWN. ) ;
#11617 =( REPRESENTATION_RELATIONSHIP ('NONE','NONE', #10127, #6508 ) REPRESENTATION_RELATIONSHIP_WITH_TRANSFORMATION ( #19592 )SHAPE_REPRESENTATION_RELATIONSHIP( ) );
#11618 = CIRCLE ( 'NONE', #14674, 2.500000000000002220 ) ;
#11619 = DIRECTION ( 'NONE',  ( -1.110223024625157172E-14, 0.000000000000000000, -1.000000000000000000 ) ) ;
#11620 = AXIS2_PLACEMENT_3D ( 'NONE', #20449, #5845, #18739 ) ;
#11621 = DIRECTION ( 'NONE',  ( -1.000000000000000000, -0.000000000000000000, -0.000000000000000000 ) ) ;
#11622 = AXIS2_PLACEMENT_3D ( 'NONE', #13649, #4044, #20587 ) ;
#11623 = ORIENTED_EDGE ( 'NONE', *, *, #10933, .F. ) ;
#11624 = EDGE_CURVE ( 'NONE', #3113, #22598, #14034, .T. ) ;
#11625 = EDGE_LOOP ( 'NONE', ( #8711, #3212, #16149, #7850 ) ) ;
#11626 = DIRECTION ( 'NONE',  ( -0.000000000000000000, -0.000000000000000000, 1.000000000000000000 ) ) ;
#11627 = FACE_OUTER_BOUND ( 'NONE', #18043, .T. ) ;
#11628 = ADVANCED_FACE ( 'NONE', ( #1068 ), #948, .F. ) ;
#11629 = ORIENTED_EDGE ( 'NONE', *, *, #8544, .F. ) ;
#11630 = CARTESIAN_POINT ( 'NONE',  ( -5.040301471719076609, -5.750234626350520628, -0.09933465333851741741 ) ) ;
#11631 = EDGE_CURVE ( 'NONE', #4056, #19785, #7544, .T. ) ;
#11632 = LINE ( 'NONE', #7730, #19159 ) ;
#11633 = AXIS2_PLACEMENT_3D ( 'NONE', #3612, #1809, #18356 ) ;
#11634 = ORIENTED_EDGE ( 'NONE', *, *, #11891, .F. ) ;
#11635 = FACE_OUTER_BOUND ( 'NONE', #16033, .T. ) ;
#11636 = AXIS2_PLACEMENT_3D ( 'NONE', #22796, #10138, #22899 ) ;
#11637 = VECTOR ( 'NONE', #5846, 1000.000000000000000 ) ;
#11638 = ORIENTED_EDGE ( 'NONE', *, *, #12300, .T. ) ;
#11639 = PLANE ( 'NONE',  #13338 ) ;
#11640 = ORIENTED_EDGE ( 'NONE', *, *, #16063, .T. ) ;
#11641 = ORIENTED_EDGE ( 'NONE', *, *, #8742, .T. ) ;
#11642 = FACE_BOUND ( 'NONE', #21865, .T. ) ;
#11643 = CARTESIAN_POINT ( 'NONE',  ( -285.2000000000013529, -89.99999999999896261, -42.98333333333330586 ) ) ;
#11644 = LINE ( 'NONE', #23016, #17886 ) ;
#11645 = CARTESIAN_POINT ( 'NONE',  ( -281.3429506979391590, 269.5484459290825043, -145.6225751257467778 ) ) ;
#11646 = CARTESIAN_POINT ( 'NONE',  ( 22.47082401081927827, -988.9212198408001768, 145.0000119999999981 ) ) ;
#11647 = CARTESIAN_POINT ( 'NONE',  ( 155.0000000000000284, -500.0000000000000000, 30.00000000000001421 ) ) ;
#11648 = CARTESIAN_POINT ( 'NONE',  ( 281.4928932188134354, -129.2000000000000455, -152.4000000000012847 ) ) ;
#11649 = ORIENTED_EDGE ( 'NONE', *, *, #18345, .T. ) ;
#11650 = DIRECTION ( 'NONE',  ( 1.000000000000000000, 0.000000000000000000, 0.000000000000000000 ) ) ;
#11651 = CARTESIAN_POINT ( 'NONE',  ( -2.411464220262952818, -7.267994521134228059, -7.491772860715828486 ) ) ;
#11652 = VERTEX_POINT ( 'NONE', #6870 ) ;
#11653 = CARTESIAN_POINT ( 'NONE',  ( -136.6960319176259588, -1073.069888270694719, -31.65816015360259428 ) ) ;
#11654 = DIRECTION ( 'NONE',  ( 1.000000000000000000, 0.000000000000000000, -0.000000000000000000 ) ) ;
#11655 = ORIENTED_EDGE ( 'NONE', *, *, #9719, .F. ) ;
#11656 = EDGE_CURVE ( 'NONE', #9824, #22116, #18251, .T. ) ;
#11657 = DIRECTION ( 'NONE',  ( -1.000000000000000000, 0.000000000000000000, 0.000000000000000000 ) ) ;
#11658 = ORIENTED_EDGE ( 'NONE', *, *, #11412, .F. ) ;
#11659 = CARTESIAN_POINT ( 'NONE',  ( 2.500000000000002220, -3.469446951953614189E-15, -2.041999999999998483 ) ) ;
#11660 = CARTESIAN_POINT ( 'NONE',  ( 279.9999999999999432, 273.0000000000000000, -144.9999999999999716 ) ) ;
#11661 = ORIENTED_EDGE ( 'NONE', *, *, #19638, .F. ) ;
#11662 = CARTESIAN_POINT ( 'NONE',  ( -281.2440776823446527, 268.3679143846943020, 147.1132285165672329 ) ) ;
#11663 = EDGE_CURVE ( 'NONE', #23309, #15457, #21828, .T. ) ;
#11664 = ORIENTED_EDGE ( 'NONE', *, *, #21870, .F. ) ;
#11665 = LINE ( 'NONE', #22367, #19899 ) ;
#11666 = ORIENTED_EDGE ( 'NONE', *, *, #6702, .F. ) ;
#11667 = DIRECTION ( 'NONE',  ( 1.000000000000000000, 3.495664435217746987E-15, 0.000000000000000000 ) ) ;
#11668 = CARTESIAN_POINT ( 'NONE',  ( 6.874999999999999112, 4.690970937165706900, -7.298562697733104621 ) ) ;
#11669 = DIRECTION ( 'NONE',  ( 1.000000000000000000, 0.000000000000000000, 0.000000000000000000 ) ) ;
#11670 = CARTESIAN_POINT ( 'NONE',  ( -288.2000000000006708, 90.00000000000100897, 32.35000000000001563 ) ) ;
#11671 = ORIENTED_EDGE ( 'NONE', *, *, #19929, .T. ) ;
#11672 = CARTESIAN_POINT ( 'NONE',  ( -281.4928932188134354, 267.7999999999999545, -150.1999999999999318 ) ) ;
#11673 =( LENGTH_UNIT ( ) NAMED_UNIT ( * ) SI_UNIT ( .MILLI., .METRE. ) );
#11675 = ORIENTED_EDGE ( 'NONE', *, *, #12197, .T. ) ;
#11674 = ORIENTED_EDGE ( 'NONE', *, *, #20103, .T. ) ;
#11676 = CARTESIAN_POINT ( 'NONE',  ( 163.0000000000002274, -210.0000000000003411, -29.99999999999344880 ) ) ;
#11677 = CARTESIAN_POINT ( 'NONE',  ( -281.4928932188135491, -127.0000000000000568, 152.4000000000014268 ) ) ;
#11678 = CARTESIAN_POINT ( 'NONE',  ( 44.80746418436846312, -137.9031948627969655, 90.00000000000000000 ) ) ;
#11679 = CARTESIAN_POINT ( 'NONE',  ( 279.9999999999999432, 272.9999999999999432, 145.0000000000000284 ) ) ;
#11680 = ADVANCED_FACE ( 'NONE', ( #11002 ), #12710, .T. ) ;
#11681 = CYLINDRICAL_SURFACE ( 'NONE', #5641, 4.250000000000000000 ) ;
#11682 = ORIENTED_EDGE ( 'NONE', *, *, #11412, .T. ) ;
#11683 = CARTESIAN_POINT ( 'NONE',  ( -281.4928932188135491, -129.2000000000000455, 150.2000000000013813 ) ) ;
#11684 = CARTESIAN_POINT ( 'NONE',  ( -44.80746418436748968, 137.9031948627972781, -90.00000000000000000 ) ) ;
#11685 = CARTESIAN_POINT ( 'NONE',  ( 123.4696136271390685, -1093.703085459772637, 28.11170275877346114 ) ) ;
#11686 = ADVANCED_FACE ( 'NONE', ( #7215 ), #2445, .T. ) ;
#11687 = EDGE_CURVE ( 'NONE', #4754, #2497, #16060, .T. ) ;
#11688 = CONTEXT_DEPENDENT_SHAPE_REPRESENTATION ( #20016, #6397 ) ;
#11689 = ORIENTED_EDGE ( 'NONE', *, *, #1195, .T. ) ;
#11690 = CARTESIAN_POINT ( 'NONE',  ( 0.000000000000000000, 0.000000000000000000, 125.0000000000000284 ) ) ;
#11691 = VERTEX_POINT ( 'NONE', #19668 ) ;
#11692 = DIRECTION ( 'NONE',  ( 0.000000000000000000, 0.000000000000000000, 1.000000000000000000 ) ) ;
#11693 = DIRECTION ( 'NONE',  ( -0.000000000000000000, -0.000000000000000000, -1.000000000000000000 ) ) ;
#11694 = EDGE_LOOP ( 'NONE', ( #6394, #8170, #12944, #16934 ) ) ;
#11695 = DIRECTION ( 'NONE',  ( 0.8090169943749552228, -0.5877852522924623679, 0.000000000000000000 ) ) ;
#11696 = VERTEX_POINT ( 'NONE', #3130 ) ;
#11697 = DIRECTION ( 'NONE',  ( 0.000000000000000000, 0.000000000000000000, -1.000000000000000000 ) ) ;
#11698 = CARTESIAN_POINT ( 'NONE',  ( -1.312671235360383548, -3.860931062424228788, -0.05923475698271369466 ) ) ;
#11699 = DIRECTION ( 'NONE',  ( -1.000000000000000000, -0.000000000000000000, -0.000000000000000000 ) ) ;
#11700 = EDGE_CURVE ( 'NONE', #23656, #19450, #17861, .T. ) ;
#11701 = FACE_OUTER_BOUND ( 'NONE', #8732, .T. ) ;
#11702 = DIRECTION ( 'NONE',  ( 1.000000000000000000, 0.000000000000000000, 0.000000000000000000 ) ) ;
#11703 = CARTESIAN_POINT ( 'NONE',  ( -4.211140560182196957, -2.431303136016552013, -3.745885042887436178 ) ) ;
#11704 = CARTESIAN_POINT ( 'NONE',  ( -24.99999999999999289, 1.636246173744676291, 145.0000119999999697 ) ) ;
#11705 = ORIENTED_EDGE ( 'NONE', *, *, #13234, .F. ) ;
#11706 = CARTESIAN_POINT ( 'NONE',  ( 5.000000000000000000, 2.342598717236902939, -4.057500000000001883 ) ) ;
#11707 = DIRECTION ( 'NONE',  ( -1.110223024625157172E-14, 0.000000000000000000, -1.000000000000000000 ) ) ;
#11708 = ORIENTED_EDGE ( 'NONE', *, *, #17996, .F. ) ;
#11709 = VECTOR ( 'NONE', #8192, 1000.000000000000000 ) ;
#11710 = EDGE_LOOP ( 'NONE', ( #17766, #169 ) ) ;
#11711 = CARTESIAN_POINT ( 'NONE',  ( 0.000000000000000000, 0.000000000000000000, -150.0000000000000000 ) ) ;
#11712 = CARTESIAN_POINT ( 'NONE',  ( -79.99999999999997158, -62.00000000000001421, 5.199999999999997513 ) ) ;
#11713 = CARTESIAN_POINT ( 'NONE',  ( 281.7484459290825498, 269.1429506979392841, -145.8703180930665155 ) ) ;
#11714 = ORIENTED_EDGE ( 'NONE', *, *, #5633, .F. ) ;
#11715 = CARTESIAN_POINT ( 'NONE',  ( 2.500000000000000000, 0.000000000000000000, 0.000000000000000000 ) ) ;
#11716 = DIRECTION ( 'NONE',  ( -0.000000000000000000, -0.000000000000000000, -1.000000000000000000 ) ) ;
#11717 = EDGE_CURVE ( 'NONE', #4643, #8989, #13304, .T. ) ;
#11718 = DIRECTION ( 'NONE',  ( 1.000000000000000000, 0.000000000000000000, 0.000000000000000000 ) ) ;
#11719 = EDGE_CURVE ( 'NONE', #13438, #2480, #8633, .T. ) ;
#11720 = ORIENTED_EDGE ( 'NONE', *, *, #9487, .F. ) ;
#11721 = CARTESIAN_POINT ( 'NONE',  ( 4.211140560182196957, -2.431303136016555122, -3.745885042887436622 ) ) ;
#11722 = CARTESIAN_POINT ( 'NONE',  ( -282.2000000000010687, -19.99999999999898392, 107.6499999999999631 ) ) ;
#11723 = EDGE_CURVE ( 'NONE', #17692, #13438, #10190, .T. ) ;
#11724 = B_SPLINE_CURVE_WITH_KNOTS ( 'NONE', 3,
 ( #6253, #21090, #13659, #10241, #17119, #12090, #4546, #17582 ),
 .UNSPECIFIED., .F., .F.,
 ( 4, 2, 2, 4 ),
 ( 2.465131517071352357E-07, 0.001183067374689843057, 0.001774477805458910071, 0.002365888236227977302 ),
 .UNSPECIFIED. ) ;
#11725 = DIRECTION ( 'NONE',  ( 0.000000000000000000, -1.000000000000000000, 0.000000000000000000 ) ) ;
#11726 = EDGE_LOOP ( 'NONE', ( #1983, #20920, #17484, #23644 ) ) ;
#11727 = PLANE ( 'NONE',  #23130 ) ;
#11728 = VECTOR ( 'NONE', #7462, 1000.000000000000000 ) ;
#11729 = ITEM_DEFINED_TRANSFORMATION ( 'NONE', 'NONE', #5787,  #11210 ) ;
#11730 = DIRECTION ( 'NONE',  ( -0.000000000000000000, -0.000000000000000000, -1.000000000000000000 ) ) ;
#11731 = EDGE_CURVE ( 'NONE', #12943, #6907, #21951, .T. ) ;
#11732 = EDGE_CURVE ( 'NONE', #5401, #20231, #16212, .T. ) ;
#11733 = DIRECTION ( 'NONE',  ( -0.5877852522924773560, 0.8090169943749444537, 0.000000000000000000 ) ) ;
#11734 = CARTESIAN_POINT ( 'NONE',  ( 281.4928932188133786, 269.9999999999999432, 150.1999999999999886 ) ) ;
#11735 = UNCERTAINTY_MEASURE_WITH_UNIT (LENGTH_MEASURE( 1.000000000000000082E-05 ), #18533, 'distance_accuracy_value', 'NONE');
#11736 = VERTEX_POINT ( 'NONE', #6999 ) ;
#11737 = ORIENTED_EDGE ( 'NONE', *, *, #3708, .F. ) ;
#11738 = DIRECTION ( 'NONE',  ( 1.000000000000000000, 0.000000000000000000, 0.000000000000000000 ) ) ;
#11739 = CARTESIAN_POINT ( 'NONE',  ( -117.3074641843669781, -85.22886158240918064, -90.00000000000000000 ) ) ;
#11740 = PRESENTATION_LAYER_ASSIGNMENT (  '', '', ( #7853 ) ) ;
#11741 = CIRCLE ( 'NONE', #11336, 2.041999999999999815 ) ;
#11742 = APPLICATION_CONTEXT ( 'automotive_design' ) ;
#11743 = ORIENTED_EDGE ( 'NONE', *, *, #3209, .T. ) ;
#11744 = LINE ( 'NONE', #3851, #19097 ) ;
#11745 = CARTESIAN_POINT ( 'NONE',  ( -127.2684398464544415, 88.47467185906430132, 32.24990070396069086 ) ) ;
#11746 = ORIENTED_EDGE ( 'NONE', *, *, #16496, .T. ) ;
#11747 = CARTESIAN_POINT ( 'NONE',  ( 2.500000000000000000, 2.357898499370432166, -2.385244779468109755E-15 ) ) ;
#11748 = EDGE_LOOP ( 'NONE', ( #22934, #3500 ) ) ;
#11749 = CARTESIAN_POINT ( 'NONE',  ( 0.2500000000000002220, 0.000000000000000000, 0.000000000000000000 ) ) ;
#11750 = FACE_OUTER_BOUND ( 'NONE', #19172, .T. ) ;
#11751 = ORIENTED_EDGE ( 'NONE', *, *, #16705, .T. ) ;
#11752 = ORIENTED_EDGE ( 'NONE', *, *, #5098, .F. ) ;
#11753 = CARTESIAN_POINT ( 'NONE',  ( 153.5653415408403646, -1122.352966361445169, 32.50000000000675726 ) ) ;
#11754 = DIRECTION ( 'NONE',  ( 0.000000000000000000, 0.000000000000000000, -1.000000000000000000 ) ) ;
#11755 = AXIS2_PLACEMENT_3D ( 'NONE', #18897, #2224, #22634 ) ;
#11756 = ADVANCED_FACE ( 'NONE', ( #18324 ), #18216, .F. ) ;
#11757 = ADVANCED_FACE ( 'NONE', ( #23408 ), #23542, .F. ) ;
#11758 = CARTESIAN_POINT ( 'NONE',  ( -40.00000000000000000, 100.0000000000000000, 150.2000000000009550 ) ) ;
#11759 = CARTESIAN_POINT ( 'NONE',  ( 15.24974479720504661, -980.1223093604610312, 145.0000119999999697 ) ) ;
#11760 = DIRECTION ( 'NONE',  ( -1.000000000000000000, 0.000000000000000000, -0.000000000000000000 ) ) ;
#11761 = ORIENTED_EDGE ( 'NONE', *, *, #20454, .F. ) ;
#11762 = CARTESIAN_POINT ( 'NONE',  ( -6.658902113226115027, -5.287118297636088649, -7.776713651266535798 ) ) ;
#11763 = SURFACE_STYLE_FILL_AREA ( #729 ) ;
#11764 = VERTEX_POINT ( 'NONE', #14387 ) ;
#11765 = FACE_OUTER_BOUND ( 'NONE', #23126, .T. ) ;
#11766 = CARTESIAN_POINT ( 'NONE',  ( 3.510273485745307731, 2.827716139362654424, -3.610536846335885564 ) ) ;
#11767 = ORIENTED_EDGE ( 'NONE', *, *, #20225, .T. ) ;
#11768 = VECTOR ( 'NONE', #9133, 1000.000000000000000 ) ;
#11769 = CARTESIAN_POINT ( 'NONE',  ( -1.641270926519074580, -24.99999999999990763, -145.0000000000000000 ) ) ;
#11770 = AXIS2_PLACEMENT_3D ( 'NONE', #282, #7519, #1837 ) ;
#11771 = ORIENTED_EDGE ( 'NONE', *, *, #6020, .T. ) ;
#11772 = CARTESIAN_POINT ( 'NONE',  ( -6.373714457846809652E-15, -56.79999999999976978, 75.17098115668784430 ) ) ;
#11773 = CONICAL_SURFACE ( 'NONE', #6773, 2.055000000000001492, 0.7853981633974633780 ) ;
#11774 = CARTESIAN_POINT ( 'NONE',  ( 283.1682701916305405, 271.9268706878665967, -145.6222583006964726 ) ) ;
#11775 = ORIENTED_EDGE ( 'NONE', *, *, #4602, .T. ) ;
#11776 = CARTESIAN_POINT ( 'NONE',  ( -280.9952621458756994, 270.4339272673396977, 149.5699028110927884 ) ) ;
#11777 = CARTESIAN_POINT ( 'NONE',  ( 90.00000000000000000, -149.9999999999996874, 129.9038105676659711 ) ) ;
#11778 = ORIENTED_EDGE ( 'NONE', *, *, #6502, .F. ) ;
#11779 = B_SPLINE_CURVE_WITH_KNOTS ( 'NONE', 3,
 ( #12198, #21329, #14354, #19746, #21686, #10606, #10357, #1274, #17705, #8653, #1167, #8541, #16025, #23373, #6833, #7423, #20457, #13149, #3783, #9488 ),
 .UNSPECIFIED., .F., .F.,
 ( 4, 2, 2, 2, 2, 2, 2, 2, 2, 4 ),
 ( 0.000000000000000000, 0.001035985217005822284, 0.002071970434011644567, 0.003107955651017466851, 0.003625948259520370403, 0.004143940868023274389, 0.005179926085028964400, 0.006215911302034655278, 0.007251896519040346156, 0.008287881736046037034 ),
 .UNSPECIFIED. ) ;
#11780 = FACE_OUTER_BOUND ( 'NONE', #22422, .T. ) ;
#11781 = AXIS2_PLACEMENT_3D ( 'NONE', #6086, #7422, #2093 ) ;
#11782 = CARTESIAN_POINT ( 'NONE',  ( -37.61698748598514896, -140.0355749532212428, -90.00000000000000000 ) ) ;
#11783 = DIRECTION ( 'NONE',  ( 0.000000000000000000, 0.000000000000000000, -1.000000000000000000 ) ) ;
#11784 = CIRCLE ( 'NONE', #3618, 4.250000000000000000 ) ;
#11785 = CIRCLE ( 'NONE', #19057, 0.2500000000000002220 ) ;
#11786 = CARTESIAN_POINT ( 'NONE',  ( -288.2000000000008981, 35.00000000000100897, 105.0000000000000000 ) ) ;
#11787 = ORIENTED_EDGE ( 'NONE', *, *, #13943, .F. ) ;
#11788 = CARTESIAN_POINT ( 'NONE',  ( -281.2440776823445390, 269.1689414351990308, -150.0938770989752697 ) ) ;
#11789 = VECTOR ( 'NONE', #6660, 1000.000000000000000 ) ;
#11791 = VERTEX_POINT ( 'NONE', #14491 ) ;
#11790 = VERTEX_POINT ( 'NONE', #23646 ) ;
#11792 = VECTOR ( 'NONE', #11075, 1000.000000000000000 ) ;
#11793 = DIRECTION ( 'NONE',  ( 1.000000000000000000, -1.408839003528726857E-14, -6.982962677686266711E-15 ) ) ;
#11794 = CARTESIAN_POINT ( 'NONE',  ( 4.000000000000000000, -2.309401076758514915, -3.433295621305383349 ) ) ;
#11795 = DIRECTION ( 'NONE',  ( -1.000000000000000000, 0.000000000000000000, 0.000000000000000000 ) ) ;
#11796 = CARTESIAN_POINT ( 'NONE',  ( 281.3610889986682082, 272.8646579186752774, 145.2488155364688964 ) ) ;
#11797 = CARTESIAN_POINT ( 'NONE',  ( -40.33333333333332860, -89.99999999999997158, 3.000000000000001332 ) ) ;
#11798 = VERTEX_POINT ( 'NONE', #1560 ) ;
#11799 = FACE_OUTER_BOUND ( 'NONE', #7325, .T. ) ;
#11800 = VECTOR ( 'NONE', #17238, 1000.000000000000000 ) ;
#11801 = DIRECTION ( 'NONE',  ( 1.000000000000000000, 0.000000000000000000, 0.000000000000000000 ) ) ;
#11802 = DIRECTION ( 'NONE',  ( -1.000000000000000000, -0.000000000000000000, -0.000000000000000000 ) ) ;
#11803 = CONTEXT_DEPENDENT_SHAPE_REPRESENTATION ( #12207, #12047 ) ;
#11804 = EDGE_CURVE ( 'NONE', #18225, #12392, #1921, .T. ) ;
#11805 = VERTEX_POINT ( 'NONE', #7107 ) ;
#11806 = CIRCLE ( 'NONE', #6771, 7.499999999999996447 ) ;
#11807 = DIRECTION ( 'NONE',  ( 1.000000000000000000, 0.000000000000000000, 0.000000000000000000 ) ) ;
#11808 = ORIENTED_EDGE ( 'NONE', *, *, #2934, .F. ) ;
#11809 = CARTESIAN_POINT ( 'NONE',  ( -79.99999999999995737, -138.0000000000000284, 0.000000000000000000 ) ) ;
#11810 = CARTESIAN_POINT ( 'NONE',  ( 0.000000000000000000, 0.000000000000000000, 90.00000000000000000 ) ) ;
#11811 = ORIENTED_EDGE ( 'NONE', *, *, #19160, .T. ) ;
#11812 = CARTESIAN_POINT ( 'NONE',  ( -22.46869086674645288, 11.08405874231984001, -145.0000000000000000 ) ) ;
#11813 = EDGE_LOOP ( 'NONE', ( #17897, #6225, #19204, #15871 ) ) ;
#11814 = LINE ( 'NONE', #14937, #6911 ) ;
#11815 = DIRECTION ( 'NONE',  ( 0.000000000000000000, 0.000000000000000000, 1.000000000000000000 ) ) ;
#11816 = EDGE_CURVE ( 'NONE', #8393, #21826, #148, .T. ) ;
#11817 = LINE ( 'NONE', #10440, #9642 ) ;
#11818 = DIRECTION ( 'NONE',  ( 1.000000000000000000, 0.000000000000000000, 0.000000000000000000 ) ) ;
#11819 = CARTESIAN_POINT ( 'NONE',  ( -59.99999999999996447, 1.678138721159888895E-29, 4.479364028612180224E-15 ) ) ;
#11820 = AXIS2_PLACEMENT_3D ( 'NONE', #18680, #8089, #20505 ) ;
#11821 = EDGE_CURVE ( 'NONE', #6807, #9294, #4765, .T. ) ;
#11822 = CARTESIAN_POINT ( 'NONE',  ( -0.6920835326022555245, -4.454600218803899558, -3.597382984111586079 ) ) ;
#11823 = ADVANCED_FACE ( 'NONE', ( #3702 ), #10963, .F. ) ;
#11824 = LINE ( 'NONE', #17459, #5135 ) ;
#11825 = EDGE_LOOP ( 'NONE', ( #23170, #1441 ) ) ;
#11826 =( NAMED_UNIT ( * ) PLANE_ANGLE_UNIT ( ) SI_UNIT ( $, .RADIAN. ) );
#11827 = FACE_OUTER_BOUND ( 'NONE', #2020, .T. ) ;
#11828 = DIRECTION ( 'NONE',  ( -1.000000000000000000, 1.408839003528726857E-14, 6.982962677686266711E-15 ) ) ;
#11829 = EDGE_CURVE ( 'NONE', #5111, #16275, #11119, .T. ) ;
#11830 = ORIENTED_EDGE ( 'NONE', *, *, #13093, .T. ) ;
#11831 = MECHANICAL_DESIGN_GEOMETRIC_PRESENTATION_REPRESENTATION (  '', ( #15268 ), #962 ) ;
#11832 = ORIENTED_EDGE ( 'NONE', *, *, #21176, .T. ) ;
#11833 = CIRCLE ( 'NONE', #7535, 160.0000000000000000 ) ;
#11834 = CARTESIAN_POINT ( 'NONE',  ( 5.000000000000015099, 0.000000000000000000, 0.000000000000000000 ) ) ;
#11835 = DIRECTION ( 'NONE',  ( 0.000000000000000000, 1.000000000000000000, 1.177509268541832635E-16 ) ) ;
#11837 = DIRECTION ( 'NONE',  ( -0.000000000000000000, 1.000000000000000000, -0.000000000000000000 ) ) ;
#11836 = PRODUCT_DEFINITION_SHAPE ( 'NONE', 'NONE',  #23870 ) ;
#11838 = VECTOR ( 'NONE', #15062, 1000.000000000000000 ) ;
#11839 = CARTESIAN_POINT ( 'NONE',  ( 131.7935180829127830, 81.58110848117821945, 31.53271418707680240 ) ) ;
#11840 = DIRECTION ( 'NONE',  ( -6.753181414994864868E-15, 6.753181414994864868E-15, -1.000000000000000000 ) ) ;
#11841 = CARTESIAN_POINT ( 'NONE',  ( 2.500000000000000000, 0.000000000000000000, 0.000000000000000000 ) ) ;
#11842 = VERTEX_POINT ( 'NONE', #9656 ) ;
#11843 = CARTESIAN_POINT ( 'NONE',  ( 4.198928548860774157, -0.8158838809860124996, -3.526471437616918170 ) ) ;
#11844 = CIRCLE ( 'NONE', #14143, 7.500000000000001776 ) ;
#11845 = CARTESIAN_POINT ( 'NONE',  ( 155.0000000000000568, -1000.000000000000000, -90.00000000000000000 ) ) ;
#11846 = DIRECTION ( 'NONE',  ( -1.350636282998972974E-14, 0.000000000000000000, -1.000000000000000000 ) ) ;
#11847 = VERTEX_POINT ( 'NONE', #18923 ) ;
#11848 = FACE_OUTER_BOUND ( 'NONE', #9816, .T. ) ;
#11849 = CIRCLE ( 'NONE', #18339, 0.4000000000000001887 ) ;
#11850 = ITEM_DEFINED_TRANSFORMATION ( 'NONE', 'NONE', #16575,  #11210 ) ;
#11851 = PLANE ( 'NONE',  #5765 ) ;
#11852 = DIRECTION ( 'NONE',  ( 1.000000000000000000, -1.408839003528726857E-14, -6.982962677686266711E-15 ) ) ;
#11853 = FACE_OUTER_BOUND ( 'NONE', #4156, .T. ) ;
#11854 = EDGE_CURVE ( 'NONE', #15819, #19218, #6310, .T. ) ;
#11855 = EDGE_LOOP ( 'NONE', ( #4953, #13125, #1437, #17303 ) ) ;
#11856 = ORIENTED_EDGE ( 'NONE', *, *, #23674, .T. ) ;
#11857 = DIRECTION ( 'NONE',  ( 1.000000000000000000, 0.000000000000000000, 0.000000000000000000 ) ) ;
#11858 = AXIS2_PLACEMENT_3D ( 'NONE', #9251, #16615, #14692 ) ;
#11859 = LINE ( 'NONE', #14980, #15259 ) ;
#11860 = EDGE_CURVE ( 'NONE', #21513, #1763, #17017, .T. ) ;
#11861 = ORIENTED_EDGE ( 'NONE', *, *, #15487, .F. ) ;
#11862 = EDGE_CURVE ( 'NONE', #14993, #15297, #7456, .T. ) ;
#11863 = VERTEX_POINT ( 'NONE', #13413 ) ;
#11864 = CARTESIAN_POINT ( 'NONE',  ( 2.500000000000002220, 2.357898499370434386, -3.469446951953614189E-15 ) ) ;
#11865 = EDGE_CURVE ( 'NONE', #21387, #21376, #22887, .T. ) ;
#11866 = CARTESIAN_POINT ( 'NONE',  ( -25.00000000000001776, 45.00100000000062295, 124.9999999999998579 ) ) ;
#11867 = EDGE_CURVE ( 'NONE', #12500, #6504, #22538, .T. ) ;
#11868 = ORIENTED_EDGE ( 'NONE', *, *, #3404, .F. ) ;
#11869 = PLANE ( 'NONE',  #4442 ) ;
#11870 = VERTEX_POINT ( 'NONE', #13060 ) ;
#11871 = AXIS2_PLACEMENT_3D ( 'NONE', #9937, #20907, #11890 ) ;
#11872 = LINE ( 'NONE', #19181, #16416 ) ;
#11873 = CARTESIAN_POINT ( 'NONE',  ( 0.000000000000000000, 0.000000000000000000, -25.03750572909317285 ) ) ;
#11874 = CARTESIAN_POINT ( 'NONE',  ( -7.500000000000000000, 4.330127018922191873, -0.9999999999999970024 ) ) ;
#11875 = EDGE_LOOP ( 'NONE', ( #15019, #14021, #3463, #203 ) ) ;
#11876 = ORIENTED_EDGE ( 'NONE', *, *, #558, .F. ) ;
#11877 = CARTESIAN_POINT ( 'NONE',  ( 2.756197834950227410, 3.027510591568626896, -3.223146290109805356 ) ) ;
#11878 = DIRECTION ( 'NONE',  ( -1.000000000000000000, 0.000000000000000000, 0.000000000000000000 ) ) ;
#11879 = CARTESIAN_POINT ( 'NONE',  ( 1.305263714129178743, -8.377797850839291627, -7.792447862505339273 ) ) ;
#11880 = CARTESIAN_POINT ( 'NONE',  ( 285.2000000000008981, 9.892604858775018348E-13, 0.000000000000000000 ) ) ;
#11881 = ORIENTED_EDGE ( 'NONE', *, *, #6674, .F. ) ;
#11882 = CARTESIAN_POINT ( 'NONE',  ( -5.174575781537456010, -5.672711317431625488, -7.030005583190790830 ) ) ;
#11883 =( LENGTH_UNIT ( ) NAMED_UNIT ( * ) SI_UNIT ( .MILLI., .METRE. ) );
#11884 = VECTOR ( 'NONE', #16920, 1000.000000000000000 ) ;
#11885 = MANIFOLD_SOLID_BREP ( 'M5 Clearance Hole1', #11023 ) ;
#11886 = ORIENTED_EDGE ( 'NONE', *, *, #17470, .F. ) ;
#11887 = VECTOR ( 'NONE', #15700, 1000.000000000000000 ) ;
#11888 = PLANE ( 'NONE',  #2603 ) ;
#11889 = EDGE_LOOP ( 'NONE', ( #10179, #9121, #23239, #1571 ) ) ;
#11890 = DIRECTION ( 'NONE',  ( 0.000000000000000000, 0.000000000000000000, -1.000000000000000000 ) ) ;
#11891 = EDGE_CURVE ( 'NONE', #17932, #21974, #16652, .T. ) ;
#11892 = EDGE_CURVE ( 'NONE', #21528, #13636, #19790, .T. ) ;
#11893 = EDGE_LOOP ( 'NONE', ( #1086, #21393, #5454, #10224 ) ) ;
#11895 = EDGE_CURVE ( 'NONE', #9258, #3739, #11610, .T. ) ;
#11894 = DIRECTION ( 'NONE',  ( 5.758888509154132365E-17, 0.7071067811865489050, 0.7071067811865462405 ) ) ;
#11896 = CARTESIAN_POINT ( 'NONE',  ( 2.500000000000000000, -1.178949249685213863, 2.042000000000001148 ) ) ;
#11897 = ORIENTED_EDGE ( 'NONE', *, *, #17558, .T. ) ;
#11898 = CARTESIAN_POINT ( 'NONE',  ( -281.3684665762326063, 268.0840560642351988, 147.1696999999999775 ) ) ;
#11899 = DIRECTION ( 'NONE',  ( 1.000000000000000000, 0.000000000000000000, 0.000000000000000000 ) ) ;
#11900 = ORIENTED_EDGE ( 'NONE', *, *, #17205, .T. ) ;
#11901 = UNCERTAINTY_MEASURE_WITH_UNIT (LENGTH_MEASURE( 1.000000000000000082E-05 ), #18586, 'distance_accuracy_value', 'NONE');
#11902 = DIRECTION ( 'NONE',  ( 5.551115123125785858E-15, 0.000000000000000000, -1.000000000000000000 ) ) ;
#11903 = AXIS2_PLACEMENT_3D ( 'NONE', #16587, #20077, #22004 ) ;
#11904 = DIRECTION ( 'NONE',  ( 1.000000000000000000, 0.000000000000000000, 0.000000000000000000 ) ) ;
#11905 = PLANE ( 'NONE',  #20355 ) ;
#11906 = VECTOR ( 'NONE', #5461, 1000.000000000000000 ) ;
#11907 = DIRECTION ( 'NONE',  ( 0.000000000000000000, 0.000000000000000000, -1.000000000000000000 ) ) ;
#11908 = ORIENTED_EDGE ( 'NONE', *, *, #6493, .T. ) ;
#11909 = DIRECTION ( 'NONE',  ( -0.000000000000000000, -0.000000000000000000, 1.000000000000000000 ) ) ;
#11910 = PRESENTATION_STYLE_ASSIGNMENT (( #20805 ) ) ;
#11912 = EDGE_LOOP ( 'NONE', ( #792, #2434, #4831, #13660, #20777 ) ) ;
#11911 = VERTEX_POINT ( 'NONE', #2013 ) ;
#11913 = DIRECTION ( 'NONE',  ( 1.000000000000000000, -1.408839003528726857E-14, -6.982962677686266711E-15 ) ) ;
#11914 = CARTESIAN_POINT ( 'NONE',  ( 7.499999999999999112, 0.7577384720672989404, -7.446470314338469620 ) ) ;
#11915 = CARTESIAN_POINT ( 'NONE',  ( 131.7919310846384633, 81.58367163796934562, -31.52881987646414430 ) ) ;
#11916 = VECTOR ( 'NONE', #13398, 1000.000000000000000 ) ;
#11917 = B_SPLINE_CURVE_WITH_KNOTS ( 'NONE', 3,
 ( #23372, #14001, #6606, #4430, #21328, #1026, #14112, #12315, #11839, #2952, #19145, #4784, #23136, #6473, #2607, #19622, #10004, #4544, #15910, #3090, #15790, #19380, #13885, #19502, #2840, #2741, #17369, #10491 ),
 .UNSPECIFIED., .F., .F.,
 ( 4, 2, 2, 2, 2, 2, 2, 2, 2, 2, 2, 2, 2, 4 ),
 ( 0.007862850516742146689, 0.008354729399060715003, 0.008846608281379283317, 0.009830366046016426884, 0.01032224492833498306, 0.01081412381065353923, 0.01130600269297209540, 0.01179788157529065157, 0.01278163933992775350, 0.01327351822224631314, 0.01376539710456487625, 0.01425727598688343763, 0.01474915486920199900, 0.01573291263383916339 ),
 .UNSPECIFIED. ) ;
#11918 = LINE ( 'NONE', #2807, #15039 ) ;
#11919 = LINE ( 'NONE', #19232, #4866 ) ;
#11920 = EDGE_CURVE ( 'NONE', #12317, #6379, #4002, .T. ) ;
#11921 = EDGE_LOOP ( 'NONE', ( #19427, #19001, #9677, #16520 ) ) ;
#11922 = VECTOR ( 'NONE', #22632, 1000.000000000000000 ) ;
#11923 = CARTESIAN_POINT ( 'NONE',  ( -45.00000000000000000, 272.9999999999999432, 5.249999999999991118 ) ) ;
#11924 = CIRCLE ( 'NONE', #4959, 145.0000000000000284 ) ;
#11925 = EDGE_CURVE ( 'NONE', #784, #10443, #23145, .T. ) ;
#11926 = ADVANCED_BREP_SHAPE_REPRESENTATION ( '', ( #19817, #11210 ), #17342 ) ;
#11927 = FACE_OUTER_BOUND ( 'NONE', #23686, .T. ) ;
#11928 = CARTESIAN_POINT ( 'NONE',  ( 124.4701338314437891, -1092.369831568442805, 27.50000000000646239 ) ) ;
#11929 = ITEM_DEFINED_TRANSFORMATION ( 'NONE', 'NONE', #14294,  #11210 ) ;
#11930 = VERTEX_POINT ( 'NONE', #4321 ) ;
#11931 = CARTESIAN_POINT ( 'NONE',  ( -155.0000000000000284, -1000.000000000000000, -90.00000000000000000 ) ) ;
#11932 = EDGE_LOOP ( 'NONE', ( #17176, #1976, #10041, #15121 ) ) ;
#11933 = DIRECTION ( 'NONE',  ( 0.000000000000000000, 0.000000000000000000, 1.000000000000000000 ) ) ;
#11934 = DIRECTION ( 'NONE',  ( -1.000000000000000000, 3.051161311199799893E-31, 8.144298233840332611E-17 ) ) ;
#11935 = VERTEX_POINT ( 'NONE', #8074 ) ;
#11936 = CARTESIAN_POINT ( 'NONE',  ( 21.69904058246457268, 12.52399064369876669, -145.0000000000000000 ) ) ;
#11937 = EDGE_LOOP ( 'NONE', ( #19998, #3320, #21710, #6430 ) ) ;
#11938 = CARTESIAN_POINT ( 'NONE',  ( -31.74999999999995737, 0.000000000000000000, 4.250000000000000000 ) ) ;
#11939 = CARTESIAN_POINT ( 'NONE',  ( 89.00000000000000000, -149.9999999999996874, 129.9038105676659711 ) ) ;
#11940 = CARTESIAN_POINT ( 'NONE',  ( 34.75000000000005684, 100.0000000000000000, -147.2000000000005571 ) ) ;
#11941 = AXIS2_PLACEMENT_3D ( 'NONE', #10674, #1457, #21750 ) ;
#11942 = CARTESIAN_POINT ( 'NONE',  ( 282.1999999999999318, 267.7999999999999545, 146.4928932188134922 ) ) ;
#11943 = LINE ( 'NONE', #15431, #15422 ) ;
#11944 = AXIS2_PLACEMENT_3D ( 'NONE', #11010, #20609, #16531 ) ;
#11945 = CARTESIAN_POINT ( 'NONE',  ( -90.00000000000000000, -94.99999999999998579, 0.000000000000000000 ) ) ;
#11946 = VECTOR ( 'NONE', #2795, 1000.000000000000000 ) ;
#11947 = ORIENTED_EDGE ( 'NONE', *, *, #3655, .F. ) ;
#11948 = DIRECTION ( 'NONE',  ( 1.000000000000000000, 0.000000000000000000, 0.000000000000000000 ) ) ;
#11949 = CARTESIAN_POINT ( 'NONE',  ( 107.6499999999999773, 35.00000000000000000, 3.000000000000001332 ) ) ;
#11950 = CIRCLE ( 'NONE', #9673, 5.249999999999973355 ) ;
#11951 = VERTEX_POINT ( 'NONE', #23011 ) ;
#11952 = ADVANCED_FACE ( 'NONE', ( #20868, #15456, #4553, #22661, #4438 ), #10367, .T. ) ;
#11953 = ORIENTED_EDGE ( 'NONE', *, *, #26, .T. ) ;
#11954 = LINE ( 'NONE', #1021, #23087 ) ;
#11955 = EDGE_CURVE ( 'NONE', #14819, #18629, #15981, .T. ) ;
#11956 = CARTESIAN_POINT ( 'NONE',  ( -35.00000000000001421, 90.00000000000001421, 3.000000000000000000 ) ) ;
#11957 = CARTESIAN_POINT ( 'NONE',  ( 155.0000000000000284, 2.775557561562891351E-16, -90.00000000000000000 ) ) ;
#11958 = VECTOR ( 'NONE', #15179, 1000.000000000000000 ) ;
#11960 = CIRCLE ( 'NONE', #6892, 7.500000000000000000 ) ;
#11959 =( GEOMETRIC_REPRESENTATION_CONTEXT ( 3 ) GLOBAL_UNCERTAINTY_ASSIGNED_CONTEXT ( ( #2383 ) ) GLOBAL_UNIT_ASSIGNED_CONTEXT ( ( #20647, #17050, #19193 ) ) REPRESENTATION_CONTEXT ( 'NONE', 'WORKASPACE' ) );
#11961 = AXIS2_PLACEMENT_3D ( 'NONE', #2737, #6956, #10487 ) ;
#11962 = DIRECTION ( 'NONE',  ( 0.000000000000000000, 0.000000000000000000, 1.000000000000000000 ) ) ;
#11963 = DIRECTION ( 'NONE',  ( 0.000000000000000000, 0.000000000000000000, 1.000000000000000000 ) ) ;
#11964 = ADVANCED_FACE ( 'NONE', ( #9890 ), #10246, .T. ) ;
#11965 = VECTOR ( 'NONE', #16283, 1000.000000000000114 ) ;
#11966 = AXIS2_PLACEMENT_3D ( 'NONE', #8747, #21302, #19466 ) ;
#11967 = VECTOR ( 'NONE', #4188, 1000.000000000000000 ) ;
#11968 = CYLINDRICAL_SURFACE ( 'NONE', #10035, 2.649999999999985700 ) ;
#11969 = ORIENTED_EDGE ( 'NONE', *, *, #18351, .T. ) ;
#11970 = CARTESIAN_POINT ( 'NONE',  ( 145.0000000000000568, -1000.000000000000000, -90.00000000000000000 ) ) ;
#11971 = FACE_OUTER_BOUND ( 'NONE', #4524, .T. ) ;
#11972 = EDGE_CURVE ( 'NONE', #18892, #16653, #6613, .T. ) ;
#11973 = AXIS2_PLACEMENT_3D ( 'NONE', #5039, #21571, #17581 ) ;
#11974 = CARTESIAN_POINT ( 'NONE',  ( 117.3074641843682144, -85.22886158240748955, -90.00000000000000000 ) ) ;
#11975 = VERTEX_POINT ( 'NONE', #20980 ) ;
#11976 = DIRECTION ( 'NONE',  ( 0.000000000000000000, 2.618450529776319755E-15, 1.000000000000000000 ) ) ;
#11977 = CONTEXT_DEPENDENT_SHAPE_REPRESENTATION ( #22026, #12344 ) ;
#11978 = DIRECTION ( 'NONE',  ( -1.000000000000000000, -3.469446951953598905E-16, 4.625929269271498733E-16 ) ) ;
#11979 = LINE ( 'NONE', #927, #18095 ) ;
#11980 = CARTESIAN_POINT ( 'NONE',  ( -31.74999999999995737, 3.061616997868383634E-16, -2.500000000000000444 ) ) ;
#11981 = EDGE_LOOP ( 'NONE', ( #12732, #16545 ) ) ;
#11982 = COLOUR_RGB ( '',1.000000000000000000, 0.9490196078431372140, 0.9098039215686274384 ) ;
#11983 = ORIENTED_EDGE ( 'NONE', *, *, #15374, .F. ) ;
#11984 = AXIS2_PLACEMENT_3D ( 'NONE', #3536, #20307, #3646 ) ;
#11985 = FACE_OUTER_BOUND ( 'NONE', #5887, .T. ) ;
#11986 = AXIS2_PLACEMENT_3D ( 'NONE', #11078, #9021, #5503 ) ;
#11987 = CARTESIAN_POINT ( 'NONE',  ( 144.8060344827587471, -7.497491405670203335, -2.775557561562891351E-14 ) ) ;
#11988 = AXIS2_PLACEMENT_3D ( 'NONE', #9988, #20956, #18899 ) ;
#11989 = AXIS2_PLACEMENT_3D ( 'NONE', #11507, #16914, #19069 ) ;
#11990 = ORIENTED_EDGE ( 'NONE', *, *, #20314, .F. ) ;
#11991 = CIRCLE ( 'NONE', #14287, 2.499999999999998668 ) ;
#11992 = AXIS2_PLACEMENT_3D ( 'NONE', #9651, #13409, #464 ) ;
#11993 = EDGE_LOOP ( 'NONE', ( #10694, #16184 ) ) ;
#11994 = DIRECTION ( 'NONE',  ( 0.000000000000000000, 1.000000000000000000, 0.000000000000000000 ) ) ;
#11995 = ADVANCED_FACE ( 'NONE', ( #12094 ), #2960, .F. ) ;
#11996 = CARTESIAN_POINT ( 'NONE',  ( -1.118033988749894458, 2.632990618166809235E-15, 21.50000000000000000 ) ) ;
#11997 = ORIENTED_EDGE ( 'NONE', *, *, #5134, .F. ) ;
#11998 = EDGE_CURVE ( 'NONE', #11363, #8656, #6480, .T. ) ;
#11999 = CARTESIAN_POINT ( 'NONE',  ( 0.000000000000000000, 0.000000000000000000, 200.0000000000000000 ) ) ;
#12000 = ORIENTED_EDGE ( 'NONE', *, *, #21507, .F. ) ;
#12002 = AXIS2_PLACEMENT_3D ( 'NONE', #3729, #22207, #5676 ) ;
#12001 = AXIS2_PLACEMENT_3D ( 'NONE', #1971, #7294, #9360 ) ;
#12003 = DIRECTION ( 'NONE',  ( -0.000000000000000000, -0.000000000000000000, 1.000000000000000000 ) ) ;
#12004 = EDGE_CURVE ( 'NONE', #9978, #7326, #14833, .T. ) ;
#12005 = DIRECTION ( 'NONE',  ( 1.000000000000000000, 0.000000000000000000, 0.000000000000000000 ) ) ;
#12006 = ORIENTED_EDGE ( 'NONE', *, *, #11865, .T. ) ;
#12007 = ORIENTED_EDGE ( 'NONE', *, *, #13051, .F. ) ;
#12008 = CARTESIAN_POINT ( 'NONE',  ( 4.235886605889389145, 2.417314728048528760, -3.751161874094018245 ) ) ;
#12009 = AXIS2_PLACEMENT_3D ( 'NONE', #3866, #5560, #8842 ) ;
#12010 = CIRCLE ( 'NONE', #1546, 2.055000000000001492 ) ;
#12011 = EDGE_CURVE ( 'NONE', #19824, #4421, #10207, .T. ) ;
#12012 = CARTESIAN_POINT ( 'NONE',  ( 3.522875095019493141, -2.820352903225631369, -3.598441714920572299 ) ) ;
#12013 = CARTESIAN_POINT ( 'NONE',  ( 105.0000000000000000, -19.99999999999998934, 3.000000000000000000 ) ) ;
#12014 = AXIS2_PLACEMENT_3D ( 'NONE', #6256, #13189, #6006 ) ;
#12015 = ORIENTED_EDGE ( 'NONE', *, *, #7182, .F. ) ;
#12016 = CARTESIAN_POINT ( 'NONE',  ( 89.00000000000000000, -94.99999999999998579, 0.000000000000000000 ) ) ;
#12017 =( NAMED_UNIT ( * ) SI_UNIT ( $, .STERADIAN. ) SOLID_ANGLE_UNIT ( ) );
#12018 = MANIFOLD_SOLID_BREP ( 'Cut-Extrude-Thin1', #7929 ) ;
#12019 = EDGE_LOOP ( 'NONE', ( #19316, #5992, #8962, #21742 ) ) ;
#12020 = AXIS2_PLACEMENT_3D ( 'NONE', #18247, #11162, #12983 ) ;
#12021 = AXIS2_PLACEMENT_3D ( 'NONE', #7751, #12695, #208 ) ;
#12022 = VECTOR ( 'NONE', #8221, 1000.000000000000000 ) ;
#12023 = AXIS2_PLACEMENT_3D ( 'NONE', #16610, #1620, #23710 ) ;
#12024 = EDGE_LOOP ( 'NONE', ( #20994, #3079, #12986, #4236 ) ) ;
#12025 = DIRECTION ( 'NONE',  ( 0.000000000000000000, -1.000000000000000000, -5.286776307738891306E-15 ) ) ;
#12026 = ORIENTED_EDGE ( 'NONE', *, *, #17558, .F. ) ;
#12027 = DIRECTION ( 'NONE',  ( 0.000000000000000000, 0.4999999999999991118, -0.8660254037844391517 ) ) ;
#12028 = DIRECTION ( 'NONE',  ( -1.000000000000000000, -0.000000000000000000, -0.000000000000000000 ) ) ;
#12029 = ORIENTED_EDGE ( 'NONE', *, *, #2841, .F. ) ;
#12030 = ADVANCED_FACE ( 'NONE', ( #21094 ), #19280, .F. ) ;
#12031 = DIRECTION ( 'NONE',  ( 0.000000000000000000, 0.000000000000000000, -1.000000000000000000 ) ) ;
#12032 = LINE ( 'NONE', #4970, #21777 ) ;
#12033 = EDGE_CURVE ( 'NONE', #22116, #11293, #19635, .T. ) ;
#12034 = EDGE_LOOP ( 'NONE', ( #6437, #9759, #3804, #23410 ) ) ;
#12035 = EDGE_CURVE ( 'NONE', #4834, #6737, #9052, .T. ) ;
#12036 = DIRECTION ( 'NONE',  ( -0.000000000000000000, -0.000000000000000000, 1.000000000000000000 ) ) ;
#12037 = ORIENTED_EDGE ( 'NONE', *, *, #21790, .F. ) ;
#12038 = EDGE_CURVE ( 'NONE', #12593, #10284, #5047, .T. ) ;
#12039 = LINE ( 'NONE', #9949, #10175 ) ;
#12040 = DIRECTION ( 'NONE',  ( 1.000000000000000000, 0.000000000000000000, 0.000000000000000000 ) ) ;
#12041 = ADVANCED_FACE ( 'NONE', ( #21693 ), #10498, .T. ) ;
#12042 = LINE ( 'NONE', #22727, #18825 ) ;
#12043 = ORIENTED_EDGE ( 'NONE', *, *, #17351, .F. ) ;
#12044 = DIRECTION ( 'NONE',  ( 0.000000000000000000, 0.000000000000000000, -1.000000000000000000 ) ) ;
#12045 = EDGE_CURVE ( 'NONE', #907, #12356, #19752, .T. ) ;
#12046 = FILL_AREA_STYLE ('',( #4626 ) ) ;
#12047 = PRODUCT_DEFINITION_SHAPE ( 'NONE', 'NONE',  #23847 ) ;
#12049 = EDGE_LOOP ( 'NONE', ( #11538, #21814, #1254, #3170 ) ) ;
#12048 = ORIENTED_EDGE ( 'NONE', *, *, #4428, .T. ) ;
#12050 = DIRECTION ( 'NONE',  ( 0.000000000000000000, 0.000000000000000000, 1.000000000000000000 ) ) ;
#12051 = CARTESIAN_POINT ( 'NONE',  ( -109.8074641843669781, -85.22886158240918064, -90.00000000000000000 ) ) ;
#12052 = LINE ( 'NONE', #988, #6581 ) ;
#12053 = DIRECTION ( 'NONE',  ( 0.000000000000000000, 0.000000000000000000, 1.000000000000000000 ) ) ;
#12054 = FACE_OUTER_BOUND ( 'NONE', #10384, .T. ) ;
#12055 = CARTESIAN_POINT ( 'NONE',  ( -281.3520027839448971, 269.5592670532759030, -145.6220388411722126 ) ) ;
#12056 = VERTEX_POINT ( 'NONE', #18189 ) ;
#12057 = MANIFOLD_SOLID_BREP ( 'Hex', #15648 ) ;
#12058 = CARTESIAN_POINT ( 'NONE',  ( -107.6499999999999773, 30.00000000000001421, 3.000000000000000000 ) ) ;
#12059 = EDGE_CURVE ( 'NONE', #7634, #21672, #9424, .T. ) ;
#12060 = LINE ( 'NONE', #4393, #6895 ) ;
#12061 = SURFACE_SIDE_STYLE ('',( #3054 ) ) ;
#12062 = CONTEXT_DEPENDENT_SHAPE_REPRESENTATION ( #4148, #8538 ) ;
#12063 = ORIENTED_EDGE ( 'NONE', *, *, #11141, .T. ) ;
#12064 = PLANE ( 'NONE',  #1329 ) ;
#12065 = ORIENTED_EDGE ( 'NONE', *, *, #17834, .T. ) ;
#12066 = DIRECTION ( 'NONE',  ( -0.000000000000000000, -0.000000000000000000, 1.000000000000000000 ) ) ;
#12067 = CARTESIAN_POINT ( 'NONE',  ( 45.00000000000002132, -59.79999999999933635, 197.6500000000002331 ) ) ;
#12068 = ORIENTED_EDGE ( 'NONE', *, *, #23489, .F. ) ;
#12069 = CARTESIAN_POINT ( 'NONE',  ( -6.487720808684898977, 24.19924082458020820, -145.0000000000000000 ) ) ;
#12070 = ORIENTED_EDGE ( 'NONE', *, *, #11366, .T. ) ;
#12071 = DIRECTION ( 'NONE',  ( 0.000000000000000000, -1.000000000000000000, 0.000000000000000000 ) ) ;
#12072 = CARTESIAN_POINT ( 'NONE',  ( -7.908030677224553884, 3.059924800338342799, -7.792662696733364314 ) ) ;
#12073 = DIRECTION ( 'NONE',  ( 0.000000000000000000, 0.000000000000000000, 1.000000000000000000 ) ) ;
#12074 = EDGE_CURVE ( 'NONE', #20363, #21672, #16032, .T. ) ;
#12075 = CARTESIAN_POINT ( 'NONE',  ( 3.678949249685231848, 0.000000000000000000, -6.938893903907228378E-15 ) ) ;
#12076 = EDGE_CURVE ( 'NONE', #11790, #12773, #14240, .T. ) ;
#12077 = FACE_OUTER_BOUND ( 'NONE', #16886, .T. ) ;
#12078 = CARTESIAN_POINT ( 'NONE',  ( 45.24999999999994316, 100.0000000000000000, -147.2000000000005571 ) ) ;
#12079 = ORIENTED_EDGE ( 'NONE', *, *, #12603, .T. ) ;
#12080 =( NAMED_UNIT ( * ) PLANE_ANGLE_UNIT ( ) SI_UNIT ( $, .RADIAN. ) );
#12081 = FACE_OUTER_BOUND ( 'NONE', #17807, .T. ) ;
#12082 = CARTESIAN_POINT ( 'NONE',  ( -4.211399284164270895, 2.459729995988205964, -3.751162237960538715 ) ) ;
#12083 = ORIENTED_EDGE ( 'NONE', *, *, #20234, .F. ) ;
#12084 = ORIENTED_EDGE ( 'NONE', *, *, #3808, .T. ) ;
#12085 = CARTESIAN_POINT ( 'NONE',  ( 2.500000000000002220, -2.357898499370430834, 3.469446951953614189E-15 ) ) ;
#12086 = CARTESIAN_POINT ( 'NONE',  ( 126.3653543294811499, 77.28387428943223370, 32.05500000000641592 ) ) ;
#12087 = CYLINDRICAL_SURFACE ( 'NONE', #13726, 4.250000000000000000 ) ;
#12088 = DIRECTION ( 'NONE',  ( 1.000000000000000000, 0.000000000000000000, 0.000000000000000000 ) ) ;
#12089 = DIRECTION ( 'NONE',  ( 0.000000000000000000, 0.000000000000000000, 1.000000000000000000 ) ) ;
#12090 = CARTESIAN_POINT ( 'NONE',  ( -2.345747346278108214, 3.264484291692489215, -0.01223254789873409049 ) ) ;
#12091 = EDGE_LOOP ( 'NONE', ( #400, #4947, #17257, #3126 ) ) ;
#12092 = CARTESIAN_POINT ( 'NONE',  ( 25.00000000000004263, -37.41657386773938754, 35.00000000000013500 ) ) ;
#12093 = CARTESIAN_POINT ( 'NONE',  ( -1.500000000000000000, 9.886859966642589370, 200.0000119999999981 ) ) ;
#12094 = FACE_OUTER_BOUND ( 'NONE', #983, .T. ) ;
#12095 = ORIENTED_EDGE ( 'NONE', *, *, #8114, .T. ) ;
#12096 = DIRECTION ( 'NONE',  ( 0.000000000000000000, 1.000000000000000000, 0.000000000000000000 ) ) ;
#12097 = MANIFOLD_SOLID_BREP ( 'EndChamfer', #3644 ) ;
#12098 = CARTESIAN_POINT ( 'NONE',  ( -90.00000000000000000, -149.9999999999996874, 129.9038105676659711 ) ) ;
#12099 = DIRECTION ( 'NONE',  ( 1.000000000000000000, 0.000000000000000000, 0.000000000000000000 ) ) ;
#12100 = FACE_OUTER_BOUND ( 'NONE', #1465, .T. ) ;
#12101 = CARTESIAN_POINT ( 'NONE',  ( 2.500000000000000000, 0.000000000000000000, 0.000000000000000000 ) ) ;
#12102 = AXIS2_PLACEMENT_3D ( 'NONE', #15450, #2247, #9761 ) ;
#12103 = VERTEX_POINT ( 'NONE', #22509 ) ;
#12104 = ORIENTED_EDGE ( 'NONE', *, *, #9418, .F. ) ;
#12105 = DIRECTION ( 'NONE',  ( 1.000000000000000000, 0.000000000000000000, 0.000000000000000000 ) ) ;
#12106 = CARTESIAN_POINT ( 'NONE',  ( 2.500000000000000000, 2.357898499370433054, -1.951563910473907981E-15 ) ) ;
#12107 = VERTEX_POINT ( 'NONE', #22039 ) ;
#12108 = ORIENTED_EDGE ( 'NONE', *, *, #8444, .T. ) ;
#12109 = DIRECTION ( 'NONE',  ( -0.000000000000000000, -1.177509268541832635E-16, 1.000000000000000000 ) ) ;
#12110 = DIRECTION ( 'NONE',  ( 1.000000000000000000, -1.408839003528726857E-14, -6.982962677686266711E-15 ) ) ;
#12111 = VERTEX_POINT ( 'NONE', #11327 ) ;
#12112 = CARTESIAN_POINT ( 'NONE',  ( -135.6313030678085170, -1075.027834699370487, -27.51562286569267002 ) ) ;
#12113 = ORIENTED_EDGE ( 'NONE', *, *, #4490, .T. ) ;
#12114 = CARTESIAN_POINT ( 'NONE',  ( 37.61698748598716691, -140.0355749532207028, 90.00000000000000000 ) ) ;
#12115 = CARTESIAN_POINT ( 'NONE',  ( -7.897836333153808397, -1.530409084195006653, -7.633857274177628938 ) ) ;
#12116 = ORIENTED_EDGE ( 'NONE', *, *, #9758, .F. ) ;
#12117 = VERTEX_POINT ( 'NONE', #8548 ) ;
#12118 = CARTESIAN_POINT ( 'NONE',  ( 133.0106877214038832, 79.58129789419575673, -27.51610016701188499 ) ) ;
#12119 = LINE ( 'NONE', #10055, #18128 ) ;
#12120 = CARTESIAN_POINT ( 'NONE',  ( -37.30746418436748968, 137.9031948627972781, -90.00000000000000000 ) ) ;
#12121 = DIRECTION ( 'NONE',  ( 1.000000000000000000, 0.000000000000000000, -0.000000000000000000 ) ) ;
#12122 = EDGE_CURVE ( 'NONE', #4872, #9091, #2460, .T. ) ;
#12123 = ORIENTED_EDGE ( 'NONE', *, *, #11065, .F. ) ;
#12124 = CARTESIAN_POINT ( 'NONE',  ( 7.499999999999997335, 34.18698582794336005, 100.0000000000000000 ) ) ;
#12125 = EDGE_CURVE ( 'NONE', #9739, #15982, #14818, .T. ) ;
#12126 = EDGE_CURVE ( 'NONE', #23349, #19049, #9831, .T. ) ;
#12127 = ORIENTED_EDGE ( 'NONE', *, *, #15643, .T. ) ;
#12128 = EDGE_CURVE ( 'NONE', #23060, #5418, #22267, .T. ) ;
#12129 = EDGE_LOOP ( 'NONE', ( #2154, #22010, #9458, #17968 ) ) ;
#12130 = CARTESIAN_POINT ( 'NONE',  ( -40.00000000000000000, 100.0000000000000000, -150.2000000000005571 ) ) ;
#12131 = ORIENTED_EDGE ( 'NONE', *, *, #2636, .F. ) ;
#12132 = FACE_OUTER_BOUND ( 'NONE', #5284, .T. ) ;
#12133 = DIRECTION ( 'NONE',  ( -0.000000000000000000, -0.000000000000000000, 1.000000000000000000 ) ) ;
#12134 = TOROIDAL_SURFACE ( 'NONE', #5165, 4.000000000000000000, 0.2500000000000000000 ) ;
#12135 = ORIENTED_EDGE ( 'NONE', *, *, #8582, .T. ) ;
#12136 = PRODUCT_DEFINITION_SHAPE ( 'NONE', 'NONE',  #17442 ) ;
#12137=STYLED_ITEM('',(#23906),#12378);
#12138 = CARTESIAN_POINT ( 'NONE',  ( -280.9952621458756994, 268.9079617568158938, 146.9223300543793584 ) ) ;
#12139 = DIRECTION ( 'NONE',  ( -1.000000000000000000, 1.408839003528726857E-14, 6.982962677686266711E-15 ) ) ;
#12140 = VERTEX_POINT ( 'NONE', #14703 ) ;
#12141 = CARTESIAN_POINT ( 'NONE',  ( -44.99999999999997868, -56.79999999999936477, 195.0000000000001705 ) ) ;
#12142 = PLANE ( 'NONE',  #10754 ) ;
#12143 = DIRECTION ( 'NONE',  ( -1.000000000000000000, -0.000000000000000000, -0.000000000000000000 ) ) ;
#12144 = ORIENTED_EDGE ( 'NONE', *, *, #7701, .F. ) ;
#12145 = CARTESIAN_POINT ( 'NONE',  ( 34.55500000000001393, 3.061616997868384127E-16, -2.500000000000000888 ) ) ;
#12146 =( LENGTH_UNIT ( ) NAMED_UNIT ( * ) SI_UNIT ( .MILLI., .METRE. ) );
#12147 = AXIS2_PLACEMENT_3D ( 'NONE', #3232, #17982, #9300 ) ;
#12148 = EDGE_CURVE ( 'NONE', #2548, #1663, #19055, .T. ) ;
#12150 = ORIENTED_EDGE ( 'NONE', *, *, #10670, .T. ) ;
#12149 = ORIENTED_EDGE ( 'NONE', *, *, #2815, .F. ) ;
#12151 = CONICAL_SURFACE ( 'NONE', #1688, 2.055000000000001492, 0.7853981633974633780 ) ;
#12152 = DIRECTION ( 'NONE',  ( 2.832769448823989808E-16, -1.000000000000000000, 3.469446951953613794E-15 ) ) ;
#12153 = CARTESIAN_POINT ( 'NONE',  ( -2.700000000000001066, 3.061616997868383043E-15, 25.00000000000000000 ) ) ;
#12154 = CARTESIAN_POINT ( 'NONE',  ( 7.499999999999999112, 41.99999999999998579, 100.0000000000000000 ) ) ;
#12155 = EDGE_CURVE ( 'NONE', #7557, #23656, #11784, .T. ) ;
#12156 = CARTESIAN_POINT ( 'NONE',  ( -135.4018704341557964, 51.87806360044768894, 90.00000000000000000 ) ) ;
#12157 = EDGE_CURVE ( 'NONE', #8521, #12818, #16984, .T. ) ;
#12158 = FACE_OUTER_BOUND ( 'NONE', #22805, .T. ) ;
#12159 = DIRECTION ( 'NONE',  ( 1.000000000000000000, 0.000000000000000000, -0.000000000000000000 ) ) ;
#12160 = EDGE_LOOP ( 'NONE', ( #5906, #17247, #22055, #2707 ) ) ;
#12161 = FACE_OUTER_BOUND ( 'NONE', #1334, .T. ) ;
#12162 = EDGE_CURVE ( 'NONE', #17788, #8566, #13029, .T. ) ;
#12163 = ORIENTED_EDGE ( 'NONE', *, *, #6326, .T. ) ;
#12164 = PRODUCT_DEFINITION ( 'UNKNOWN', '', #2322, #1789 ) ;
#12165 = CARTESIAN_POINT ( 'NONE',  ( -7.499999999999999112, 41.99999999999998579, 100.0000000000000000 ) ) ;
#12166 = EDGE_CURVE ( 'NONE', #3521, #16653, #23302, .T. ) ;
#12167 = CARTESIAN_POINT ( 'NONE',  ( 2.500000000000000000, -1.178949249685213863, 2.042000000000002924 ) ) ;
#12168 = EDGE_LOOP ( 'NONE', ( #1536, #2085, #4390, #4273 ) ) ;
#12170 = CARTESIAN_POINT ( 'NONE',  ( 0.1756481739660539498, -4.720212674038995360, -3.469390959564070620 ) ) ;
#12169 = PRESENTATION_LAYER_ASSIGNMENT (  '', '', ( #15609 ) ) ;
#12171 = ORIENTED_EDGE ( 'NONE', *, *, #5467, .T. ) ;
#12172 = FACE_OUTER_BOUND ( 'NONE', #7594, .T. ) ;
#12173 = AXIS2_PLACEMENT_3D ( 'NONE', #4298, #17562, #21311 ) ;
#12174 = CYLINDRICAL_SURFACE ( 'NONE', #14903, 2.649999999999999467 ) ;
#12175 = ORIENTED_EDGE ( 'NONE', *, *, #13969, .T. ) ;
#12176 = PLANE ( 'NONE',  #21352 ) ;
#12177 =( NAMED_UNIT ( * ) PLANE_ANGLE_UNIT ( ) SI_UNIT ( $, .RADIAN. ) );
#12178 = CARTESIAN_POINT ( 'NONE',  ( 0.000000000000000000, 5.051668046482844583E-16, -4.000000000000000000 ) ) ;
#12179 = CARTESIAN_POINT ( 'NONE',  ( -127.9021285790841205, 87.55595642181887683, 27.50000000000646239 ) ) ;
#12180 = DIRECTION ( 'NONE',  ( 0.000000000000000000, 0.000000000000000000, 1.000000000000000000 ) ) ;
#12181 = CARTESIAN_POINT ( 'NONE',  ( 0.000000000000000000, 0.000000000000000000, -9.449444346342714240 ) ) ;
#12182 = CYLINDRICAL_SURFACE ( 'NONE', #5150, 2.500000000000000444 ) ;
#12183 = VERTEX_POINT ( 'NONE', #9375 ) ;
#12184 = PRESENTATION_STYLE_ASSIGNMENT (( #4773 ) ) ;
#12185 = CARTESIAN_POINT ( 'NONE',  ( -287.4000000000014552, -129.2000000000000455, 146.4928932188134638 ) ) ;
#12186 = DIRECTION ( 'NONE',  ( 0.5000000000000006661, 0.8660254037844383745, -0.000000000000000000 ) ) ;
#12187 = ORIENTED_EDGE ( 'NONE', *, *, #7377, .T. ) ;
#12188 = ORIENTED_EDGE ( 'NONE', *, *, #17138, .T. ) ;
#12189 = DIRECTION ( 'NONE',  ( -0.7071067811865416886, 9.961996129952529179E-15, -0.7071067811865532349 ) ) ;
#12190 = FACE_OUTER_BOUND ( 'NONE', #17387, .T. ) ;
#12191 = CYLINDRICAL_SURFACE ( 'NONE', #7125, 2.500000000000002220 ) ;
#12192 = CIRCLE ( 'NONE', #9450, 2.499999999999998668 ) ;
#12193 = AXIS2_PLACEMENT_3D ( 'NONE', #16751, #4050, #5642 ) ;
#12194 = EDGE_CURVE ( 'NONE', #3824, #22213, #1743, .T. ) ;
#12195 = EDGE_CURVE ( 'NONE', #9608, #9858, #78, .T. ) ;
#12196 = CARTESIAN_POINT ( 'NONE',  ( 5.000000000000000888, 0.000000000000000000, 0.000000000000000000 ) ) ;
#12197 = EDGE_CURVE ( 'NONE', #301, #9146, #18635, .T. ) ;
#12198 = CARTESIAN_POINT ( 'NONE',  ( -285.2000000000000455, 267.7999999999999545, -146.4928932188134354 ) ) ;
#12199 = DIRECTION ( 'NONE',  ( 0.000000000000000000, 0.000000000000000000, 1.000000000000000000 ) ) ;
#12200 = ORIENTED_EDGE ( 'NONE', *, *, #21284, .F. ) ;
#12201 = CARTESIAN_POINT ( 'NONE',  ( 287.4000000000013415, -127.0000000000000568, 146.4928932188134638 ) ) ;
#12202 = LINE ( 'NONE', #12093, #19275 ) ;
#12203 = VECTOR ( 'NONE', #19150, 1000.000000000000000 ) ;
#12204 = DIRECTION ( 'NONE',  ( 0.000000000000000000, -1.000000000000000000, -1.177509268541832635E-16 ) ) ;
#12205 = VERTEX_POINT ( 'NONE', #20217 ) ;
#12206 = DIRECTION ( 'NONE',  ( -0.000000000000000000, -1.000000000000000000, -1.110223024625156540E-16 ) ) ;
#12207 =( REPRESENTATION_RELATIONSHIP ('NONE','NONE', #10127, #19462 ) REPRESENTATION_RELATIONSHIP_WITH_TRANSFORMATION ( #6578 )SHAPE_REPRESENTATION_RELATIONSHIP( ) );
#12208 = DIRECTION ( 'NONE',  ( 0.000000000000000000, 0.000000000000000000, 1.000000000000000000 ) ) ;
#12209 = CARTESIAN_POINT ( 'NONE',  ( 0.000000000000000000, -1000.000000000000000, -90.00000000000000000 ) ) ;
#12210 = DIRECTION ( 'NONE',  ( -4.625929269271485914E-16, 3.469446951953614583E-15, 1.000000000000000000 ) ) ;
#12211 = CARTESIAN_POINT ( 'NONE',  ( 5.000000000000000000, -4.685197434473811207, 4.770489558936219510E-15 ) ) ;
#12212 = DIRECTION ( 'NONE',  ( 1.000000000000000000, 0.000000000000000000, 0.000000000000000000 ) ) ;
#12213 = CARTESIAN_POINT ( 'NONE',  ( -2.452879891156814818, -7.244083172395189507, -0.1007566405101857632 ) ) ;
#12214 = CLOSED_SHELL ( 'NONE', ( #15414, #1770, #5040, #18069, #8191, #13066, #21544, #12279, #21530, #15237, #21141, #1728, #21745, #15173, #16639, #18171, #12609, #1916, #22969, #15847, #6293, #7836, #9727, #4465, #5637, #4259, #8645, #11542 ) ) ;
#12215 = ORIENTED_EDGE ( 'NONE', *, *, #8405, .T. ) ;
#12216 = ORIENTED_EDGE ( 'NONE', *, *, #19085, .T. ) ;
#12217 = DIRECTION ( 'NONE',  ( -1.000000000000000000, -0.000000000000000000, -0.000000000000000000 ) ) ;
#12218 = LINE ( 'NONE', #11987, #3446 ) ;
#12219 = VERTEX_POINT ( 'NONE', #7431 ) ;
#12220 = CYLINDRICAL_SURFACE ( 'NONE', #9279, 145.0000000000000284 ) ;
#12221 = AXIS2_PLACEMENT_3D ( 'NONE', #11216, #3912, #548 ) ;
#12222 = ORIENTED_EDGE ( 'NONE', *, *, #10043, .T. ) ;
#12223 = PLANE ( 'NONE',  #935 ) ;
#12224 = DIRECTION ( 'NONE',  ( 0.000000000000000000, 0.4999999999999991118, -0.8660254037844391517 ) ) ;
#12225 = AXIS2_PLACEMENT_3D ( 'NONE', #16901, #15226, #11492 ) ;
#12226 = ORIENTED_EDGE ( 'NONE', *, *, #10545, .F. ) ;
#12227 = CARTESIAN_POINT ( 'NONE',  ( 80.00000000000004263, -137.9999999999999716, 0.000000000000000000 ) ) ;
#12228 = TOROIDAL_SURFACE ( 'NONE', #19492, 2.700000000000000622, 0.2000000000000000111 ) ;
#12229 = EDGE_LOOP ( 'NONE', ( #16304, #22224, #6707, #10699 ) ) ;
#12230 = LINE ( 'NONE', #10155, #21415 ) ;
#12231 = CARTESIAN_POINT ( 'NONE',  ( 155.0000000000000284, -500.0000000000000000, -32.49999999999997158 ) ) ;
#12232 = EDGE_LOOP ( 'NONE', ( #8715, #5853 ) ) ;
#12233 = ORIENTED_EDGE ( 'NONE', *, *, #10986, .T. ) ;
#12234 = CARTESIAN_POINT ( 'NONE',  ( 133.9566469371587516, 77.97836475581189575, -31.25955389945143992 ) ) ;
#12235 = PRODUCT_DEFINITION_SHAPE ( 'NONE', 'NONE',  #23830 ) ;
#12236 = CYLINDRICAL_SURFACE ( 'NONE', #17383, 5.000000000000000888 ) ;
#12237 = VECTOR ( 'NONE', #17325, 1000.000000000000114 ) ;
#12238 = CARTESIAN_POINT ( 'NONE',  ( 45.00000000000000000, 269.9999999999999432, 0.000000000000000000 ) ) ;
#12239 = CARTESIAN_POINT ( 'NONE',  ( -91.18044947428954572, 112.7436279071528844, -2.775557561562891351E-14 ) ) ;
#12240 = ORIENTED_EDGE ( 'NONE', *, *, #4893, .F. ) ;
#12241 = CARTESIAN_POINT ( 'NONE',  ( 72.64999999999999147, -112.6666666666666714, 144.9999999999999716 ) ) ;
#12242 =( LENGTH_UNIT ( ) NAMED_UNIT ( * ) SI_UNIT ( .MILLI., .METRE. ) );
#12243 = ORIENTED_EDGE ( 'NONE', *, *, #6767, .T. ) ;
#12244 = EDGE_CURVE ( 'NONE', #6121, #15650, #2103, .T. ) ;
#12245 = EDGE_LOOP ( 'NONE', ( #9860, #17059, #1669, #7251, #16058 ) ) ;
#12246 = DIRECTION ( 'NONE',  ( 0.000000000000000000, -0.000000000000000000, 1.000000000000000000 ) ) ;
#12247 = ORIENTED_EDGE ( 'NONE', *, *, #18419, .F. ) ;
#12248 = AXIS2_PLACEMENT_3D ( 'NONE', #11045, #12636, #7037 ) ;
#12249 = DIRECTION ( 'NONE',  ( -0.7071067811865320296, 9.875400524328840493E-15, 0.7071067811865631159 ) ) ;
#12250 = CARTESIAN_POINT ( 'NONE',  ( -2.000000000000006661, 3.464101615137750834, 0.000000000000000000 ) ) ;
#12251 = VERTEX_POINT ( 'NONE', #18534 ) ;
#12252 = EDGE_CURVE ( 'NONE', #19892, #15576, #7546, .T. ) ;
#12253 = DIRECTION ( 'NONE',  ( 0.000000000000000000, 0.000000000000000000, -1.000000000000000000 ) ) ;
#12254 = PLANE ( 'NONE',  #10237 ) ;
#12255 = ADVANCED_FACE ( 'NONE', ( #20464 ), #13267, .F. ) ;
#12256 = ORIENTED_EDGE ( 'NONE', *, *, #9669, .F. ) ;
#12257 = PLANE ( 'NONE',  #11212 ) ;
#12258 = DIRECTION ( 'NONE',  ( -1.000000000000000000, -2.775557561562891351E-17, 0.000000000000000000 ) ) ;
#12259 = EDGE_CURVE ( 'NONE', #10831, #23190, #4029, .T. ) ;
#12260 = AXIS2_PLACEMENT_3D ( 'NONE', #7225, #2022, #14616 ) ;
#12261 = DIRECTION ( 'NONE',  ( 0.000000000000000000, -1.000000000000000000, 9.256405414277014607E-16 ) ) ;
#12262 = PLANE ( 'NONE',  #8088 ) ;
#12263 = DIRECTION ( 'NONE',  ( -0.5877852522924643663, -0.8090169943749537795, 0.000000000000000000 ) ) ;
#12264 = EDGE_LOOP ( 'NONE', ( #3033, #3249, #14672, #5877, #2847 ) ) ;
#12265 = LINE ( 'NONE', #23793, #8860 ) ;
#12266 = CIRCLE ( 'NONE', #9148, 2.055000000000000160 ) ;
#12268 = EDGE_LOOP ( 'NONE', ( #5989, #21913, #21660, #3356 ) ) ;
#12267 = EDGE_LOOP ( 'NONE', ( #8853, #14541, #16683, #13804, #262, #5647, #2700 ) ) ;
#12269 = CARTESIAN_POINT ( 'NONE',  ( -8.339331917296304295E-16, -1000.000000000000000, -142.0000000000000284 ) ) ;
#12270 = DIRECTION ( 'NONE',  ( 0.000000000000000000, 0.000000000000000000, -1.000000000000000000 ) ) ;
#12271 = CARTESIAN_POINT ( 'NONE',  ( 4.000000000000000000, 0.1981133338132474442, 2.382280164152719704E-17 ) ) ;
#12272 = FACE_OUTER_BOUND ( 'NONE', #19847, .T. ) ;
#12273 = DIRECTION ( 'NONE',  ( -1.000000000000000000, -0.000000000000000000, -0.000000000000000000 ) ) ;
#12274 = CARTESIAN_POINT ( 'NONE',  ( -281.7350371479513456, 269.1333820183295416, -145.8708543776411659 ) ) ;
#12275 = VERTEX_POINT ( 'NONE', #9615 ) ;
#12276 = CONICAL_SURFACE ( 'NONE', #11111, 2.055000000000001492, 0.7853981633974633780 ) ;
#12277 = CARTESIAN_POINT ( 'NONE',  ( 34.99999999999999289, 0.000000000000000000, 0.000000000000000000 ) ) ;
#12278 = ORIENTED_EDGE ( 'NONE', *, *, #20313, .T. ) ;
#12279 = ADVANCED_FACE ( 'NONE', ( #441 ), #7792, .F. ) ;
#12280 = AXIS2_PLACEMENT_3D ( 'NONE', #16237, #14776, #23396 ) ;
#12281 = DIRECTION ( 'NONE',  ( 0.000000000000000000, -1.000000000000000000, -1.110223024625156540E-16 ) ) ;
#12282 =( LENGTH_UNIT ( ) NAMED_UNIT ( * ) SI_UNIT ( .MILLI., .METRE. ) );
#12283 = CONTEXT_DEPENDENT_SHAPE_REPRESENTATION ( #4302, #2530 ) ;
#12284 = ORIENTED_EDGE ( 'NONE', *, *, #16696, .F. ) ;
#12285 = LINE ( 'NONE', #23343, #2039 ) ;
#12286 = ORIENTED_EDGE ( 'NONE', *, *, #1028, .T. ) ;
#12287 = PLANE ( 'NONE',  #9641 ) ;
#12288 = CARTESIAN_POINT ( 'NONE',  ( 51.87806360044913134, -135.4018704341552564, 90.00000000000000000 ) ) ;
#12289 = EDGE_LOOP ( 'NONE', ( #13952, #3262, #9706, #14335 ) ) ;
#12290 = CARTESIAN_POINT ( 'NONE',  ( -280.9955614683503313, 270.4045710003933323, 149.5135885331258976 ) ) ;
#12291 = EDGE_CURVE ( 'NONE', #16072, #16588, #19126, .T. ) ;
#12292 = DIRECTION ( 'NONE',  ( 1.000000000000000000, 0.000000000000000000, 0.000000000000000000 ) ) ;
#12293 = CARTESIAN_POINT ( 'NONE',  ( 158.0000000000000284, -500.0000000000000000, 30.00000000000001421 ) ) ;
#12294 = EDGE_CURVE ( 'NONE', #17922, #306, #22940, .T. ) ;
#12295 = CARTESIAN_POINT ( 'NONE',  ( 0.000000000000000000, -1000.000000000000000, -138.9999999999999716 ) ) ;
#12296 = PLANE ( 'NONE',  #371 ) ;
#12297 = DIRECTION ( 'NONE',  ( -0.000000000000000000, 0.000000000000000000, -1.000000000000000000 ) ) ;
#12298 = CIRCLE ( 'NONE', #8410, 2.649999999999985700 ) ;
#12299 = DIRECTION ( 'NONE',  ( 0.000000000000000000, 1.000000000000000000, 0.000000000000000000 ) ) ;
#12300 = EDGE_CURVE ( 'NONE', #8946, #14733, #20945, .T. ) ;
#12301 = ORIENTED_EDGE ( 'NONE', *, *, #9013, .T. ) ;
#12302 = SHAPE_REPRESENTATION_RELATIONSHIP ( 'NONE' , 'NONE' ,  #22995, #17647 ) ;
#12303 = CARTESIAN_POINT ( 'NONE',  ( -146.0000000000000853, -494.4690652294807478, 30.00000000000641620 ) ) ;
#12304 = AXIS2_PLACEMENT_3D ( 'NONE', #5939, #22473, #2062 ) ;
#12305 = CARTESIAN_POINT ( 'NONE',  ( -1.500000000000000000, 11.99999999999999822, 150.0000000000000284 ) ) ;
#12306 = EDGE_CURVE ( 'NONE', #15926, #5940, #7886, .T. ) ;
#12307 = AXIS2_PLACEMENT_3D ( 'NONE', #12293, #6943, #10216 ) ;
#12308 = EDGE_LOOP ( 'NONE', ( #15592, #693, #9131, #9195 ) ) ;
#12309 = EDGE_LOOP ( 'NONE', ( #14693, #1133, #19806, #23341 ) ) ;
#12310 = AXIS2_PLACEMENT_3D ( 'NONE', #3520, #21519, #1704 ) ;
#12311 = CARTESIAN_POINT ( 'NONE',  ( 0.000000000000000000, -1000.000000000000000, 145.0000119999999697 ) ) ;
#12312 = DIRECTION ( 'NONE',  ( -1.000000000000000000, -0.000000000000000000, -0.000000000000000000 ) ) ;
#12313 = B_SPLINE_CURVE_WITH_KNOTS ( 'NONE', 3,
 ( #1102, #18136, #23565, #8722, #5210, #15973, #19815, #23316, #10673, #15733, #16217, #8598, #6783, #1585, #3151, #21282 ),
 .UNSPECIFIED., .F., .F.,
 ( 4, 2, 2, 2, 2, 2, 2, 4 ),
 ( 0.000000000000000000, 0.0009361184303672154955, 0.001404177645550738675, 0.001872236860734262072, 0.002340296075917785469, 0.002808355291101308649, 0.003276414506284832263, 0.003744473721468355443 ),
 .UNSPECIFIED. ) ;
#12314 = DIRECTION ( 'NONE',  ( -1.110223024625155594E-14, 0.000000000000000000, -1.000000000000000000 ) ) ;
#12315 = CARTESIAN_POINT ( 'NONE',  ( 131.8501689178085030, 81.48954978394043280, 31.66065886938989493 ) ) ;
#12316 = DIRECTION ( 'NONE',  ( 1.000000000000000000, -0.000000000000000000, 6.982962677686266711E-15 ) ) ;
#12317 = VERTEX_POINT ( 'NONE', #17215 ) ;
#12318 = CARTESIAN_POINT ( 'NONE',  ( -129.2206655591605511, -1072.408698320350595, 27.94500000000640227 ) ) ;
#12319 = EDGE_LOOP ( 'NONE', ( #14530, #11611, #3502, #22616 ) ) ;
#12320 = DIRECTION ( 'NONE',  ( 0.000000000000000000, -0.4999999999999992228, 0.8660254037844390407 ) ) ;
#12321 = DIRECTION ( 'NONE',  ( 1.000000000000000000, 0.000000000000000000, 0.000000000000000000 ) ) ;
#12322 = EDGE_CURVE ( 'NONE', #3739, #3608, #10109, .T. ) ;
#12323 = CIRCLE ( 'NONE', #2226, 5.249999999999949374 ) ;
#12324 = PRESENTATION_STYLE_ASSIGNMENT (( #10729 ) ) ;
#12325 = VECTOR ( 'NONE', #10282, 1000.000000000000000 ) ;
#12326 = VERTEX_POINT ( 'NONE', #19002 ) ;
#12327 = CARTESIAN_POINT ( 'NONE',  ( -282.2000000000011255, -29.99999999999898037, -105.0000000000000000 ) ) ;
#12328 = VECTOR ( 'NONE', #4027, 1000.000000000000000 ) ;
#12329 = CYLINDRICAL_SURFACE ( 'NONE', #1815, 2.500000000000002220 ) ;
#12330 = DIRECTION ( 'NONE',  ( 0.9289202219288174023, 0.3702799228849934510, 6.982962677686266711E-15 ) ) ;
#12331 = LINE ( 'NONE', #17041, #6717 ) ;
#12332 = EDGE_CURVE ( 'NONE', #3110, #10547, #19793, .T. ) ;
#12333 = CARTESIAN_POINT ( 'NONE',  ( 155.0000000000000568, -801.0618695410399823, 27.50000000000647660 ) ) ;
#12334 = DIRECTION ( 'NONE',  ( 1.000000000000000000, 0.000000000000000000, -0.000000000000000000 ) ) ;
#12335 = CARTESIAN_POINT ( 'NONE',  ( -10.12668159690567649, 1.240160820363494356E-15, -9.226681596905677907 ) ) ;
#12336 = VERTEX_POINT ( 'NONE', #21067 ) ;
#12337 = B_SPLINE_CURVE_WITH_KNOTS ( 'NONE', 3,
 ( #9391, #11101, #20004, #7562, #18421, #1880, #14954, #9283, #681, #15440 ),
 .UNSPECIFIED., .F., .F.,
 ( 4, 2, 2, 2, 4 ),
 ( 0.000000000000000000, 0.05650958017001787154, 0.1130191603400357431, 0.1695287405100536215, 0.2260383206800714861 ),
 .UNSPECIFIED. ) ;
#12339 = VERTEX_POINT ( 'NONE', #22980 ) ;
#12338 = EDGE_CURVE ( 'NONE', #5249, #5237, #16717, .T. ) ;
#12340 = CARTESIAN_POINT ( 'NONE',  ( 119.6158142514525622, -1087.367367941136990, -29.99999999999356604 ) ) ;
#12341 = CARTESIAN_POINT ( 'NONE',  ( 280.8086578304521481, 269.2538215477170525, 146.6574776399288567 ) ) ;
#12342 = ADVANCED_FACE ( 'NONE', ( #6452 ), #2353, .F. ) ;
#12343 = VERTEX_POINT ( 'NONE', #23467 ) ;
#12344 = PRODUCT_DEFINITION_SHAPE ( 'NONE', 'NONE',  #23809 ) ;
#12345 = AXIS2_PLACEMENT_3D ( 'NONE', #13299, #2133, #7710 ) ;
#12346 = DIRECTION ( 'NONE',  ( 0.000000000000000000, -1.000000000000000000, 3.469446951953614189E-15 ) ) ;
#12347 = FACE_OUTER_BOUND ( 'NONE', #11295, .T. ) ;
#12348 = VECTOR ( 'NONE', #19604, 1000.000000000000000 ) ;
#12349 = CIRCLE ( 'NONE', #1863, 10.00000000000000000 ) ;
#12350 = ORIENTED_EDGE ( 'NONE', *, *, #20155, .T. ) ;
#12351 = CARTESIAN_POINT ( 'NONE',  ( 2.500000000000000000, 2.357898499370432166, -2.385244779468109755E-15 ) ) ;
#12352 = VECTOR ( 'NONE', #7888, 1000.000000000000000 ) ;
#12353 = CARTESIAN_POINT ( 'NONE',  ( -2.699999999999997513, 0.000000000000000000, 0.000000000000000000 ) ) ;
#12354 = EDGE_LOOP ( 'NONE', ( #13183, #12419, #19063, #6089 ) ) ;
#12355 = DIRECTION ( 'NONE',  ( -1.000000000000000000, 1.408839003528726857E-14, 6.982962677686266711E-15 ) ) ;
#12356 = VERTEX_POINT ( 'NONE', #8992 ) ;
#12357 = FACE_OUTER_BOUND ( 'NONE', #8798, .T. ) ;
#12358 = DIRECTION ( 'NONE',  ( 0.000000000000000000, -0.000000000000000000, 1.000000000000000000 ) ) ;
#12359 = EDGE_LOOP ( 'NONE', ( #18032, #5942, #14545, #3187 ) ) ;
#12360 = ORIENTED_EDGE ( 'NONE', *, *, #7796, .T. ) ;
#12361 = CARTESIAN_POINT ( 'NONE',  ( 50.00000000000000000, -62.00000000000001421, 2.999999999999968914 ) ) ;
#12362 = DIRECTION ( 'NONE',  ( 1.221966984364620947E-29, 3.495664435217746987E-15, -1.000000000000000000 ) ) ;
#12364 = EDGE_CURVE ( 'NONE', #12140, #9588, #14549, .T. ) ;
#12363 =( GEOMETRIC_REPRESENTATION_CONTEXT ( 3 ) GLOBAL_UNCERTAINTY_ASSIGNED_CONTEXT ( ( #6303 ) ) GLOBAL_UNIT_ASSIGNED_CONTEXT ( ( #13864, #12177, #10336 ) ) REPRESENTATION_CONTEXT ( 'NONE', 'WORKASPACE' ) );
#12365 = DIRECTION ( 'NONE',  ( 0.000000000000000000, 1.000000000000000000, 0.000000000000000000 ) ) ;
#12366 = AXIS2_PLACEMENT_3D ( 'NONE', #5981, #13164, #18538 ) ;
#12368 = CARTESIAN_POINT ( 'NONE',  ( -1.249327701954873415, 8.410337540189265937, -7.776713651267812999 ) ) ;
#12367 = CIRCLE ( 'NONE', #374, 8.000000000000000000 ) ;
#12369 = AXIS2_PLACEMENT_3D ( 'NONE', #18987, #9481, #16835 ) ;
#12370 = CARTESIAN_POINT ( 'NONE',  ( 89.00000000000000000, -74.99999999999998579, 0.000000000000000000 ) ) ;
#12371 = PRESENTATION_LAYER_ASSIGNMENT (  '', '', ( #18476 ) ) ;
#12372 = AXIS2_PLACEMENT_3D ( 'NONE', #8412, #687, #6475 ) ;
#12373 = ORIENTED_EDGE ( 'NONE', *, *, #17140, .T. ) ;
#12374 = EDGE_CURVE ( 'NONE', #19084, #22918, #7159, .T. ) ;
#12375 = FACE_OUTER_BOUND ( 'NONE', #22943, .T. ) ;
#12376 =( NAMED_UNIT ( * ) PLANE_ANGLE_UNIT ( ) SI_UNIT ( $, .RADIAN. ) );
#12377 = EDGE_CURVE ( 'NONE', #17025, #11293, #4883, .T. ) ;
#12378 = MANIFOLD_SOLID_BREP ( 'M5 Clearance Hole1', #8697 ) ;
#12379 = ORIENTED_EDGE ( 'NONE', *, *, #21478, .T. ) ;
#12380 = EDGE_CURVE ( 'NONE', #7788, #1816, #14796, .T. ) ;
#12381 = ORIENTED_EDGE ( 'NONE', *, *, #310, .T. ) ;
#12382 = DIRECTION ( 'NONE',  ( -0.000000000000000000, -0.000000000000000000, 1.000000000000000000 ) ) ;
#12384 = VECTOR ( 'NONE', #2407, 999.9999999999997726 ) ;
#12383 = AXIS2_PLACEMENT_3D ( 'NONE', #2199, #22023, #9592 ) ;
#12385 = VERTEX_POINT ( 'NONE', #6814 ) ;
#12386 = CARTESIAN_POINT ( 'NONE',  ( 10.00000000000000000, 0.000000000000000000, -5.400000000000002132 ) ) ;
#12387 = AXIS2_PLACEMENT_3D ( 'NONE', #21351, #2979, #12346 ) ;
#12388 = VECTOR ( 'NONE', #14755, 1000.000000000000000 ) ;
#12389 = VECTOR ( 'NONE', #13786, 1000.000000000000000 ) ;
#12390 = EDGE_LOOP ( 'NONE', ( #18439, #22311, #7601, #5855 ) ) ;
#12391 = DIRECTION ( 'NONE',  ( 0.000000000000000000, 1.000000000000000000, -3.469446951953614189E-15 ) ) ;
#12392 = VERTEX_POINT ( 'NONE', #16248 ) ;
#12393 = DIRECTION ( 'NONE',  ( -1.000000000000000000, 1.408839003528726857E-14, 6.982962677686266711E-15 ) ) ;
#12394 = FACE_OUTER_BOUND ( 'NONE', #4652, .T. ) ;
#12395 = CARTESIAN_POINT ( 'NONE',  ( -59.99999999999996447, -138.3994082814338071, -3.599999999999746070 ) ) ;
#12396 = LINE ( 'NONE', #1458, #17704 ) ;
#12397 = DIRECTION ( 'NONE',  ( 1.000000000000000000, -0.000000000000000000, 6.982962677686266711E-15 ) ) ;
#12398 = ORIENTED_EDGE ( 'NONE', *, *, #23183, .T. ) ;
#12399 = DIRECTION ( 'NONE',  ( -1.110223024625155594E-14, 0.000000000000000000, -1.000000000000000000 ) ) ;
#12400 =( REPRESENTATION_RELATIONSHIP ('NONE','NONE', #10127, #22995 ) REPRESENTATION_RELATIONSHIP_WITH_TRANSFORMATION ( #19954 )SHAPE_REPRESENTATION_RELATIONSHIP( ) );
#12401 = CIRCLE ( 'NONE', #8495, 5.000000000000001776 ) ;
#12402 = EDGE_CURVE ( 'NONE', #3284, #3058, #19848, .T. ) ;
#12403 = AXIS2_PLACEMENT_3D ( 'NONE', #926, #6617, #23015 ) ;
#12404 = CIRCLE ( 'NONE', #18513, 2.499999999999998668 ) ;
#12405 = EDGE_CURVE ( 'NONE', #9588, #6149, #1258, .T. ) ;
#12407 = VERTEX_POINT ( 'NONE', #5242 ) ;
#12406 = ORIENTED_EDGE ( 'NONE', *, *, #9667, .T. ) ;
#12408 = CARTESIAN_POINT ( 'NONE',  ( -69.99999999999997158, -87.33333333333339965, 153.0000000000000000 ) ) ;
#12409 = CARTESIAN_POINT ( 'NONE',  ( -158.1195828810603246, 116.4077317428679947, 30.00000000000675726 ) ) ;
#12410 = LINE ( 'NONE', #10565, #14970 ) ;
#12411 = DIRECTION ( 'NONE',  ( 1.000000000000000000, 0.000000000000000000, -0.000000000000000000 ) ) ;
#12412 = LINE ( 'NONE', #10567, #20675 ) ;
#12413 = VERTEX_POINT ( 'NONE', #14206 ) ;
#12414 = LINE ( 'NONE', #4644, #14197 ) ;
#12415 = ORIENTED_EDGE ( 'NONE', *, *, #23452, .T. ) ;
#12416 = AXIS2_PLACEMENT_3D ( 'NONE', #1408, #15924, #12212 ) ;
#12417 = FACE_OUTER_BOUND ( 'NONE', #8797, .T. ) ;
#12418 = FACE_OUTER_BOUND ( 'NONE', #13706, .T. ) ;
#12419 = ORIENTED_EDGE ( 'NONE', *, *, #11854, .T. ) ;
#12420 = CARTESIAN_POINT ( 'NONE',  ( 17.00000000000000000, 2.516649172247811061E-16, -2.055000000000000160 ) ) ;
#12421 = VERTEX_POINT ( 'NONE', #6696 ) ;
#12422 = CARTESIAN_POINT ( 'NONE',  ( -128.6132171834563280, 86.50814704276191947, -32.17188107257626228 ) ) ;
#12423 = DIRECTION ( 'NONE',  ( 1.000000000000000000, 0.000000000000000000, 0.000000000000000000 ) ) ;
#12424 = EDGE_LOOP ( 'NONE', ( #15134, #1874 ) ) ;
#12425 = SURFACE_SIDE_STYLE ('',( #16003 ) ) ;
#12426 =( LENGTH_UNIT ( ) NAMED_UNIT ( * ) SI_UNIT ( .MILLI., .METRE. ) );
#12427 = CARTESIAN_POINT ( 'NONE',  ( 25.00000000000004974, -52.79999999999962057, 65.00000000000018474 ) ) ;
#12428 = CARTESIAN_POINT ( 'NONE',  ( 5.560781378645575757, 0.000000000000000000, -4.000000000000000000 ) ) ;
#12429 = DIRECTION ( 'NONE',  ( -0.000000000000000000, 1.000000000000000000, 0.000000000000000000 ) ) ;
#12430 = CARTESIAN_POINT ( 'NONE',  ( 29.55500000000002458, 0.000000000000000000, 2.499999999999987121 ) ) ;
#12431 = ADVANCED_FACE ( 'NONE', ( #12647 ), #12176, .T. ) ;
#12432 = FACE_BOUND ( 'NONE', #13787, .T. ) ;
#12433 = ORIENTED_EDGE ( 'NONE', *, *, #17174, .F. ) ;
#12434 = EDGE_CURVE ( 'NONE', #8692, #1257, #3296, .T. ) ;
#12435 = DIRECTION ( 'NONE',  ( -0.000000000000000000, -0.000000000000000000, 1.000000000000000000 ) ) ;
#12436 = CARTESIAN_POINT ( 'NONE',  ( 7.500000000000000000, -4.330127018922199866, -7.422398894150035176 ) ) ;
#12437 = EDGE_CURVE ( 'NONE', #12943, #1821, #1138, .T. ) ;
#12438 = EDGE_LOOP ( 'NONE', ( #18435, #15930, #5352, #1899 ) ) ;
#12439 = EDGE_LOOP ( 'NONE', ( #15025, #10103, #20613, #6834 ) ) ;
#12440 = LINE ( 'NONE', #1270, #7286 ) ;
#12441 = DIRECTION ( 'NONE',  ( 0.000000000000000000, -1.000000000000000000, 1.103561164596346103E-15 ) ) ;
#12442 = EDGE_CURVE ( 'NONE', #2692, #12111, #15500, .T. ) ;
#12443 = EDGE_CURVE ( 'NONE', #840, #2982, #16596, .T. ) ;
#12445 = CARTESIAN_POINT ( 'NONE',  ( -280.0000000000000568, 273.0299999999999159, 145.0000000000000284 ) ) ;
#12444 = PRODUCT_DEFINITION_SHAPE ( 'NONE', 'NONE',  #23857 ) ;
#12446 = CARTESIAN_POINT ( 'NONE',  ( 0.000000000000000000, 1.178949249685212086, -2.042000000000002036 ) ) ;
#12447 = CARTESIAN_POINT ( 'NONE',  ( 40.00000000000000000, 100.0000000000000000, 125.0000000000000000 ) ) ;
#12448 = ORIENTED_EDGE ( 'NONE', *, *, #7802, .F. ) ;
#12449 = CARTESIAN_POINT ( 'NONE',  ( 0.000000000000000000, 0.000000000000000000, 0.000000000000000000 ) ) ;
#12450 = ORIENTED_EDGE ( 'NONE', *, *, #12685, .T. ) ;
#12451 = CARTESIAN_POINT ( 'NONE',  ( 285.2000000000013529, -127.0000000000000568, 146.4928932188134638 ) ) ;
#12453 = EDGE_CURVE ( 'NONE', #852, #1893, #3895, .T. ) ;
#12452 = DIRECTION ( 'NONE',  ( -0.7071067811865320296, 9.875400524328840493E-15, 0.7071067811865631159 ) ) ;
#12454 = DIRECTION ( 'NONE',  ( -0.000000000000000000, -1.000000000000000000, 3.495664435217746987E-15 ) ) ;
#12455 = VERTEX_POINT ( 'NONE', #1834 ) ;
#12456 = CARTESIAN_POINT ( 'NONE',  ( 0.000000000000000000, 1.178949249685217415, 2.041999999999998483 ) ) ;
#12457 = DIRECTION ( 'NONE',  ( -1.110223024625155594E-14, 0.000000000000000000, -1.000000000000000000 ) ) ;
#12458 = DIRECTION ( 'NONE',  ( -1.000000000000000000, -2.775557561562891351E-17, 0.000000000000000000 ) ) ;
#12459 = FACE_OUTER_BOUND ( 'NONE', #4313, .T. ) ;
#12460 = LINE ( 'NONE', #10377, #10002 ) ;
#12461 = PLANE ( 'NONE',  #6519 ) ;
#12462 = CARTESIAN_POINT ( 'NONE',  ( -282.6045710003934914, 272.3135885331261079, 145.4973317504633030 ) ) ;
#12463 = VERTEX_POINT ( 'NONE', #3763 ) ;
#12464 = EDGE_LOOP ( 'NONE', ( #13646, #4776 ) ) ;
#12465 = DIRECTION ( 'NONE',  ( -0.000000000000000000, 1.000000000000000000, -3.469446951953613794E-15 ) ) ;
#12466 = CARTESIAN_POINT ( 'NONE',  ( 281.4301275412296945, 267.9452901038202413, 147.2000000000000171 ) ) ;
#12467 = ORIENTED_EDGE ( 'NONE', *, *, #706, .T. ) ;
#12468 = FACE_OUTER_BOUND ( 'NONE', #1690, .T. ) ;
#12469 = CARTESIAN_POINT ( 'NONE',  ( -2.699999999999997513, 0.000000000000000000, 0.000000000000000000 ) ) ;
#12470 = ADVANCED_FACE ( 'NONE', ( #11304 ), #11185, .F. ) ;
#12471 = VERTEX_POINT ( 'NONE', #20848 ) ;
#12472 = CARTESIAN_POINT ( 'NONE',  ( 280.6220388411721274, 271.9582675804705332, 148.1956429438695579 ) ) ;
#12473 = EDGE_CURVE ( 'NONE', #4047, #13152, #1052, .T. ) ;
#12474 = CARTESIAN_POINT ( 'NONE',  ( -40.33333333333332860, -89.99999999999997158, 0.000000000000000000 ) ) ;
#12475 = EDGE_LOOP ( 'NONE', ( #7846, #4973, #8912, #16644 ) ) ;
#12476 = EDGE_CURVE ( 'NONE', #22877, #12500, #9969, .T. ) ;
#12477 = CARTESIAN_POINT ( 'NONE',  ( 24.99999999999998579, 45.00100000000064426, 124.9999999999998579 ) ) ;
#12478 = EDGE_CURVE ( 'NONE', #8622, #20731, #9017, .T. ) ;
#12479 = ORIENTED_EDGE ( 'NONE', *, *, #21529, .F. ) ;
#12480 = EDGE_CURVE ( 'NONE', #603, #22646, #8139, .T. ) ;
#12481 = DIRECTION ( 'NONE',  ( 0.000000000000000000, 0.000000000000000000, -1.000000000000000000 ) ) ;
#12482 = EDGE_CURVE ( 'NONE', #8352, #21882, #17525, .T. ) ;
#12483 = DIRECTION ( 'NONE',  ( -1.000000000000000000, 0.000000000000000000, 0.000000000000000000 ) ) ;
#12484 = VERTEX_POINT ( 'NONE', #13716 ) ;
#12485 = VERTEX_POINT ( 'NONE', #4619 ) ;
#12486 = CARTESIAN_POINT ( 'NONE',  ( 133.8639378433822742, 78.13740870752386058, -28.46977261728505226 ) ) ;
#12487 = AXIS2_PLACEMENT_3D ( 'NONE', #18317, #16517, #1769 ) ;
#12488 = APPLICATION_PROTOCOL_DEFINITION ( 'draft international standard', 'automotive_design', 1998, #4898 ) ;
#12489 = DIRECTION ( 'NONE',  ( 0.000000000000000000, 0.000000000000000000, 1.000000000000000000 ) ) ;
#12490 = CARTESIAN_POINT ( 'NONE',  ( 126.3653543294818178, 77.28387428943173632, -29.99999999999356604 ) ) ;
#12491 = DIRECTION ( 'NONE',  ( 1.000000000000000000, -0.000000000000000000, 6.982962677686266711E-15 ) ) ;
#12492 = ORIENTED_EDGE ( 'NONE', *, *, #18547, .F. ) ;
#12493 = DIRECTION ( 'NONE',  ( 0.000000000000000000, 0.000000000000000000, 1.000000000000000000 ) ) ;
#12494 = ORIENTED_EDGE ( 'NONE', *, *, #21580, .T. ) ;
#12495 = AXIS2_PLACEMENT_3D ( 'NONE', #5434, #16310, #18567 ) ;
#12496 = ORIENTED_EDGE ( 'NONE', *, *, #14908, .T. ) ;
#12497 = CARTESIAN_POINT ( 'NONE',  ( 24.99999999999999645, -5.982013681773172432E-16, -145.0000059999999849 ) ) ;
#12498 = ORIENTED_EDGE ( 'NONE', *, *, #20501, .F. ) ;
#12499 = CARTESIAN_POINT ( 'NONE',  ( 4.174999999999999822, 0.000000000000000000, -0.5776712190230133270 ) ) ;
#12500 = VERTEX_POINT ( 'NONE', #2324 ) ;
#12501 = ADVANCED_FACE ( 'NONE', ( #4261 ), #4374, .F. ) ;
#12502 = CARTESIAN_POINT ( 'NONE',  ( -79.99999999999997158, -62.00000000000001421, 5.199999999999997513 ) ) ;
#12503 = ADVANCED_FACE ( 'NONE', ( #21035 ), #22950, .F. ) ;
#12504 = VERTEX_POINT ( 'NONE', #15385 ) ;
#12505 = DIRECTION ( 'NONE',  ( 3.469446951953614682E-16, -1.000000000000000000, 3.483493295888648978E-15 ) ) ;
#12506 = DIRECTION ( 'NONE',  ( 0.000000000000000000, 5.551115123125777969E-15, -1.000000000000000000 ) ) ;
#12507 = CONICAL_SURFACE ( 'NONE', #17874, 2.055000000000001492, 0.7853981633974633780 ) ;
#12508 = FACE_OUTER_BOUND ( 'NONE', #16185, .T. ) ;
#12509 = CARTESIAN_POINT ( 'NONE',  ( 285.1999999999999318, 267.7999999999999545, 0.000000000000000000 ) ) ;
#12510 = ORIENTED_EDGE ( 'NONE', *, *, #17385, .F. ) ;
#12511 = LINE ( 'NONE', #19821, #20713 ) ;
#12513 = ORIENTED_EDGE ( 'NONE', *, *, #8151, .T. ) ;
#12512 = ORIENTED_EDGE ( 'NONE', *, *, #13672, .F. ) ;
#12514 = DIRECTION ( 'NONE',  ( -3.469446951953613794E-15, 3.469446951953612611E-15, 1.000000000000000000 ) ) ;
#12515 = LINE ( 'NONE', #16336, #18127 ) ;
#12516 = FACE_OUTER_BOUND ( 'NONE', #7131, .T. ) ;
#12517 = CYLINDRICAL_SURFACE ( 'NONE', #14270, 10.00000000000000000 ) ;
#12518 = FACE_OUTER_BOUND ( 'NONE', #18348, .T. ) ;
#12519 = ORIENTED_EDGE ( 'NONE', *, *, #6175, .F. ) ;
#12520 = AXIS2_PLACEMENT_3D ( 'NONE', #21671, #5821, #1381 ) ;
#12521 = DIRECTION ( 'NONE',  ( -1.000000000000000000, -0.000000000000000000, -0.000000000000000000 ) ) ;
#12522 = VERTEX_POINT ( 'NONE', #525 ) ;
#12523 = CARTESIAN_POINT ( 'NONE',  ( -67.34999999999996589, -87.33333333333338544, 3.000000000000000000 ) ) ;
#12524 = CARTESIAN_POINT ( 'NONE',  ( 2.500000000000000000, -2.629050547790028551E-15, -2.041999999999999815 ) ) ;
#12525 = ITEM_DEFINED_TRANSFORMATION ( 'NONE', 'NONE', #22750,  #11210 ) ;
#12526 = VERTEX_POINT ( 'NONE', #18972 ) ;
#12527 = VERTEX_POINT ( 'NONE', #17307 ) ;
#12528 = CARTESIAN_POINT ( 'NONE',  ( 153.5653415408401941, -1122.352966361446079, -32.49999999999322853 ) ) ;
#12529 = CARTESIAN_POINT ( 'NONE',  ( -2.700000000000001510, 0.000000000000000000, 0.000000000000000000 ) ) ;
#12530 = ORIENTED_EDGE ( 'NONE', *, *, #17596, .T. ) ;
#12531 = CARTESIAN_POINT ( 'NONE',  ( -280.8083875057491241, 271.2314821058794223, 148.9107452280324537 ) ) ;
#12532 = CARTESIAN_POINT ( 'NONE',  ( 133.0100681275899035, 79.58233248384615877, 27.51597717546057353 ) ) ;
#12533 = DIRECTION ( 'NONE',  ( 0.000000000000000000, 0.000000000000000000, 1.000000000000000000 ) ) ;
#12534 = VECTOR ( 'NONE', #15350, 1000.000000000000000 ) ;
#12535 = PRODUCT_DEFINITION_SHAPE ( 'NONE', 'NONE',  #23816 ) ;
#12536 = CIRCLE ( 'NONE', #21366, 2.499999999999999556 ) ;
#12537 = DIRECTION ( 'NONE',  ( -0.7071067811865416886, 9.961996129952529179E-15, -0.7071067811865532349 ) ) ;
#12538 = CARTESIAN_POINT ( 'NONE',  ( 146.4449999999997658, -801.0618695410399823, 32.50000000000641620 ) ) ;
#12539 = CARTESIAN_POINT ( 'NONE',  ( 0.000000000000000000, 0.000000000000000000, 90.00000000000000000 ) ) ;
#12540 = DIRECTION ( 'NONE',  ( 1.000000000000000000, 0.000000000000000000, 0.000000000000000000 ) ) ;
#12541 = ORIENTED_EDGE ( 'NONE', *, *, #5727, .F. ) ;
#12542 = PRESENTATION_STYLE_ASSIGNMENT (( #16359 ) ) ;
#12543 = CARTESIAN_POINT ( 'NONE',  ( -7.500000000000000000, -4.330127018922198090, -7.422398894150034288 ) ) ;
#12544 = CARTESIAN_POINT ( 'NONE',  ( -1.257172072275743346, 3.892973519171203378, -3.433252694550776862 ) ) ;
#12545 = ORIENTED_EDGE ( 'NONE', *, *, #11443, .T. ) ;
#12546 = CARTESIAN_POINT ( 'NONE',  ( 280.2497115627124344, 269.9290760626066685, -145.5724317483736172 ) ) ;
#12547 = DIRECTION ( 'NONE',  ( 1.000000000000000000, -3.495664435217746987E-15, -0.000000000000000000 ) ) ;
#12548 = EDGE_CURVE ( 'NONE', #6763, #6579, #12039, .T. ) ;
#12549 = DIRECTION ( 'NONE',  ( 0.000000000000000000, 0.000000000000000000, -1.000000000000000000 ) ) ;
#12550 = AXIS2_PLACEMENT_3D ( 'NONE', #11974, #2747, #8304 ) ;
#12551 = VECTOR ( 'NONE', #14209, 1000.000000000000000 ) ;
#12552 = LINE ( 'NONE', #14231, #8349 ) ;
#12553 = FACE_BOUND ( 'NONE', #20692, .T. ) ;
#12554 = AXIS2_PLACEMENT_3D ( 'NONE', #1445, #22196, #5667 ) ;
#12555 = ORIENTED_EDGE ( 'NONE', *, *, #20927, .T. ) ;
#12556 = CARTESIAN_POINT ( 'NONE',  ( -90.00000000000000000, -74.99999999999998579, 0.000000000000000000 ) ) ;
#12557 = EDGE_LOOP ( 'NONE', ( #14648, #10149 ) ) ;
#12558 = EDGE_CURVE ( 'NONE', #21317, #19753, #16341, .T. ) ;
#12559 = DIRECTION ( 'NONE',  ( 0.000000000000000000, -1.000000000000000000, 0.000000000000000000 ) ) ;
#12560 = CARTESIAN_POINT ( 'NONE',  ( -90.00000000000000000, 3.053113317719180486E-13, 3.000000000000002665 ) ) ;
#12561 =( NAMED_UNIT ( * ) PLANE_ANGLE_UNIT ( ) SI_UNIT ( $, .RADIAN. ) );
#12562 = EDGE_CURVE ( 'NONE', #23739, #16727, #9798, .T. ) ;
#12563 = VERTEX_POINT ( 'NONE', #13606 ) ;
#12564 = DIRECTION ( 'NONE',  ( 3.736327486719275871E-16, -1.000000000000000000, 3.469446951953614189E-15 ) ) ;
#12565 = LINE ( 'NONE', #19876, #23036 ) ;
#12566 = DIRECTION ( 'NONE',  ( -2.775557561562891351E-17, 1.000000000000000000, 0.000000000000000000 ) ) ;
#12567 = LINE ( 'NONE', #10461, #7465 ) ;
#12568 = DIRECTION ( 'NONE',  ( 1.000000000000000000, -0.000000000000000000, 6.982962677686266711E-15 ) ) ;
#12569 = EDGE_CURVE ( 'NONE', #9373, #18998, #22599, .T. ) ;
#12570 = LINE ( 'NONE', #16384, #11965 ) ;
#12571 = DIRECTION ( 'NONE',  ( 0.000000000000000000, 0.000000000000000000, 1.000000000000000000 ) ) ;
#12572 = VERTEX_POINT ( 'NONE', #11782 ) ;
#12573 = AXIS2_PLACEMENT_3D ( 'NONE', #22503, #13379, #10208 ) ;
#12574 = ORIENTED_EDGE ( 'NONE', *, *, #12195, .T. ) ;
#12575 = DIRECTION ( 'NONE',  ( 0.000000000000000000, 1.000000000000000000, -3.495664435217746987E-15 ) ) ;
#12576 = CARTESIAN_POINT ( 'NONE',  ( 0.000000000000000000, -1.178949249685214307, 2.042000000000001592 ) ) ;
#12577 = ORIENTED_EDGE ( 'NONE', *, *, #2839, .T. ) ;
#12578 = AXIS2_PLACEMENT_3D ( 'NONE', #3501, #3376, #10667 ) ;
#12579 = VECTOR ( 'NONE', #5257, 1000.000000000000000 ) ;
#12580 = CARTESIAN_POINT ( 'NONE',  ( -1.500000000000000000, 9.886859966642592923, 0.000000000000000000 ) ) ;
#12581 = CARTESIAN_POINT ( 'NONE',  ( 5.000000000000000888, 4.250000000000000000, 0.000000000000000000 ) ) ;
#12582 = ORIENTED_EDGE ( 'NONE', *, *, #6020, .F. ) ;
#12583 = CARTESIAN_POINT ( 'NONE',  ( 281.3684637452623747, 268.4807971656551331, 150.1999999999999886 ) ) ;
#12584 = CARTESIAN_POINT ( 'NONE',  ( -102.3500000000000227, 30.00000000000001421, 3.000000000000001332 ) ) ;
#12585 = ORIENTED_EDGE ( 'NONE', *, *, #21744, .F. ) ;
#12586 = CARTESIAN_POINT ( 'NONE',  ( 60.00000000000000000, 0.000000000000000000, 0.000000000000000000 ) ) ;
#12587 = VECTOR ( 'NONE', #19663, 1000.000000000000000 ) ;
#12588 = VERTEX_POINT ( 'NONE', #19094 ) ;
#12589 = DIRECTION ( 'NONE',  ( 3.202566417187928841E-16, -1.000000000000000000, 3.469446951953614583E-15 ) ) ;
#12590 = CARTESIAN_POINT ( 'NONE',  ( 105.0000000000000000, 35.00000000000000000, 3.000000000000000000 ) ) ;
#12591 = DIRECTION ( 'NONE',  ( 1.000000000000000000, 0.000000000000000000, 0.000000000000000000 ) ) ;
#12592 = ORIENTED_EDGE ( 'NONE', *, *, #3276, .F. ) ;
#12593 = VERTEX_POINT ( 'NONE', #2558 ) ;
#12594 = CARTESIAN_POINT ( 'NONE',  ( 134.0610795706244858, 77.79865694966356671, -29.19154146838981134 ) ) ;
#12595 = AXIS2_PLACEMENT_3D ( 'NONE', #23283, #22811, #14033 ) ;
#12596 = EDGE_CURVE ( 'NONE', #14788, #20252, #17641, .T. ) ;
#12597 = CARTESIAN_POINT ( 'NONE',  ( -40.00000000000000000, 100.0000000000000000, 160.2000000000005855 ) ) ;
#12598 = CLOSED_SHELL ( 'NONE', ( #17007, #5232, #3310, #7430, #15561, #3365, #3847, #3334, #3374, #1376, #7227, #23333, #9926, #10235, #8366, #1800, #12767, #1155, #19324, #17744, #5196, #1218, #11592, #4254, #6612, #1379, #6094, #12987, #6896, #21104, #10677, #1905, #7172, #4467, #182, #17997, #6762 ) ) ;
#12599 = CARTESIAN_POINT ( 'NONE',  ( -126.4561707720353354, 89.63167338449116528, -30.32927184981475222 ) ) ;
#12600 = ADVANCED_FACE ( 'NONE', ( #12620 ), #3970, .T. ) ;
#12601 = LINE ( 'NONE', #23550, #17302 ) ;
#12602 = DIRECTION ( 'NONE',  ( 1.000000000000000000, 3.469446951953614682E-16, -0.000000000000000000 ) ) ;
#12603 = EDGE_CURVE ( 'NONE', #12593, #8982, #12313, .T. ) ;
#12604 = ORIENTED_EDGE ( 'NONE', *, *, #8582, .F. ) ;
#12605 = DIRECTION ( 'NONE',  ( -0.000000000000000000, 1.000000000000000000, 1.224646799147353207E-16 ) ) ;
#12606 = CIRCLE ( 'NONE', #13750, 20.00000000000000000 ) ;
#12607 = SURFACE_STYLE_FILL_AREA ( #7805 ) ;
#12608 = MANIFOLD_SOLID_BREP ( 'M5 Clearance Hole1', #12598 ) ;
#12609 = ADVANCED_FACE ( 'NONE', ( #12394 ), #2042, .T. ) ;
#12610 = VERTEX_POINT ( 'NONE', #23200 ) ;
#12611 = AXIS2_PLACEMENT_3D ( 'NONE', #12529, #12423, #1371 ) ;
#12612 = DIRECTION ( 'NONE',  ( 0.000000000000000000, -0.000000000000000000, -1.000000000000000000 ) ) ;
#12613 = ORIENTED_EDGE ( 'NONE', *, *, #4635, .F. ) ;
#12614 = CARTESIAN_POINT ( 'NONE',  ( -93.00000000000000000, 76.26794919243116055, 2.999999999999988898 ) ) ;
#12615 = ORIENTED_EDGE ( 'NONE', *, *, #14183, .F. ) ;
#12616 = VECTOR ( 'NONE', #19984, 1000.000000000000000 ) ;
#12617 = LINE ( 'NONE', #18470, #13341 ) ;
#12618 = ORIENTED_EDGE ( 'NONE', *, *, #18465, .T. ) ;
#12619 = LINE ( 'NONE', #12856, #12784 ) ;
#12620 = FACE_OUTER_BOUND ( 'NONE', #17270, .T. ) ;
#12621 = DIRECTION ( 'NONE',  ( 0.000000000000000000, 0.000000000000000000, 1.000000000000000000 ) ) ;
#12622 = DIRECTION ( 'NONE',  ( 0.000000000000000000, 1.224646799147353207E-16, 1.000000000000000000 ) ) ;
#12623 = DIRECTION ( 'NONE',  ( 6.580500949201931673E-15, 2.336402151923303105E-15, 1.000000000000000000 ) ) ;
#12624 = VERTEX_POINT ( 'NONE', #17890 ) ;
#12625 = FACE_OUTER_BOUND ( 'NONE', #22194, .T. ) ;
#12626 = PRODUCT_DEFINITION_SHAPE ( 'NONE', 'NONE',  #23892 ) ;
#12628 = EDGE_LOOP ( 'NONE', ( #14526, #18153 ) ) ;
#12627 = VERTEX_POINT ( 'NONE', #2899 ) ;
#12629 = DIRECTION ( 'NONE',  ( 0.000000000000000000, 0.000000000000000000, 1.000000000000000000 ) ) ;
#12630 = EDGE_CURVE ( 'NONE', #23462, #16143, #20047, .T. ) ;
#12631 = CARTESIAN_POINT ( 'NONE',  ( -109.8074641843669781, -85.22886158240918064, 90.00000000000000000 ) ) ;
#12632 = VECTOR ( 'NONE', #6569, 1000.000000000000000 ) ;
#12633 = CARTESIAN_POINT ( 'NONE',  ( 20.00000000000000000, -1000.000000000000000, 124.9999999999998579 ) ) ;
#12634 = ADVANCED_FACE ( 'NONE', ( #4852, #19563, #3024, #10438 ), #17784, .F. ) ;
#12635 = EDGE_LOOP ( 'NONE', ( #22358, #15946, #18213, #20719 ) ) ;
#12636 = DIRECTION ( 'NONE',  ( -0.000000000000000000, -0.000000000000000000, 1.000000000000000000 ) ) ;
#12637 = AXIS2_PLACEMENT_3D ( 'NONE', #21569, #17944, #8775 ) ;
#12638 = DIRECTION ( 'NONE',  ( 0.7232617928448825673, -0.6905739489807055653, -6.982962677686266711E-15 ) ) ;
#12639 = ORIENTED_EDGE ( 'NONE', *, *, #7030, .T. ) ;
#12640 = CARTESIAN_POINT ( 'NONE',  ( 105.0000000000000000, 35.00000000000000000, 3.000000000000000000 ) ) ;
#12641 = CARTESIAN_POINT ( 'NONE',  ( 80.00000000000000000, -56.79999999999998295, 5.199999999999985967 ) ) ;
#12642 = ORIENTED_EDGE ( 'NONE', *, *, #18005, .F. ) ;
#12643 = VERTEX_POINT ( 'NONE', #21640 ) ;
#12644 = CARTESIAN_POINT ( 'NONE',  ( 124.6683470056599106, -1092.102735484116010, 27.50000000000645173 ) ) ;
#12645 = ORIENTED_EDGE ( 'NONE', *, *, #20658, .F. ) ;
#12646 = CONICAL_SURFACE ( 'NONE', #2174, 2.055000000000001492, 0.7853981633974633780 ) ;
#12647 = FACE_OUTER_BOUND ( 'NONE', #929, .T. ) ;
#12648 = DIRECTION ( 'NONE',  ( -1.000000000000000000, 3.495664435217746987E-15, 0.000000000000000000 ) ) ;
#12649 = CARTESIAN_POINT ( 'NONE',  ( 1.500000000000000000, 0.000000000000000000, 200.0000000000000000 ) ) ;
#12650 = CYLINDRICAL_SURFACE ( 'NONE', #8440, 7.500000000000007105 ) ;
#12651 = LINE ( 'NONE', #3535, #20593 ) ;
#12652 = LINE ( 'NONE', #7412, #14281 ) ;
#12653 = DIRECTION ( 'NONE',  ( 1.000000000000000000, 0.000000000000000000, -0.000000000000000000 ) ) ;
#12654 = EDGE_LOOP ( 'NONE', ( #6675, #21243, #1450 ) ) ;
#12655 = EDGE_CURVE ( 'NONE', #15403, #5390, #17115, .T. ) ;
#12656 = DIRECTION ( 'NONE',  ( 1.000000000000000000, 0.000000000000000000, 0.000000000000000000 ) ) ;
#12657 = CARTESIAN_POINT ( 'NONE',  ( 2.500000000000000000, 0.000000000000000000, 0.000000000000000000 ) ) ;
#12658 = AXIS2_PLACEMENT_3D ( 'NONE', #21628, #16073, #6879 ) ;
#12659 =( REPRESENTATION_RELATIONSHIP ('NONE','NONE', #10127, #18083 ) REPRESENTATION_RELATIONSHIP_WITH_TRANSFORMATION ( #15435 )SHAPE_REPRESENTATION_RELATIONSHIP( ) );
#12660 = VERTEX_POINT ( 'NONE', #5561 ) ;
#12661 = ADVANCED_FACE ( 'NONE', ( #130, #8964 ), #5678, .T. ) ;
#12662 = CARTESIAN_POINT ( 'NONE',  ( 281.2447782964892440, 268.3743436287469990, -147.1433523009092426 ) ) ;
#12663 = FACE_OUTER_BOUND ( 'NONE', #1889, .T. ) ;
#12664 = CARTESIAN_POINT ( 'NONE',  ( -282.1132285165673466, 268.3679143846943020, 146.2440776823445105 ) ) ;
#12665 = CYLINDRICAL_SURFACE ( 'NONE', #6107, 19.99999999999999289 ) ;
#12666 = CARTESIAN_POINT ( 'NONE',  ( 281.0571358042175802, 270.1059783239181797, -149.6730547946946217 ) ) ;
#12667 = ORIENTED_EDGE ( 'NONE', *, *, #6926, .F. ) ;
#12668 = DIRECTION ( 'NONE',  ( -1.000000000000000000, 0.000000000000000000, -0.000000000000000000 ) ) ;
#12669 = VERTEX_POINT ( 'NONE', #248 ) ;
#12670 = CARTESIAN_POINT ( 'NONE',  ( -7.499999999999999112, 41.99999999999998579, 100.0000000000000000 ) ) ;
#12671 = B_SPLINE_CURVE_WITH_KNOTS ( 'NONE', 3,
 ( #16636, #7328, #11231, #14715, #11096, #91 ),
 .UNSPECIFIED., .F., .F.,
 ( 4, 2, 4 ),
 ( 0.002365888236227967761, 0.003551327329835077609, 0.004736766423442186590 ),
 .UNSPECIFIED. ) ;
#12672 = DIRECTION ( 'NONE',  ( 5.135813185032629306E-32, -1.850371707708594366E-15, -1.000000000000000000 ) ) ;
#12673 = PRESENTATION_STYLE_ASSIGNMENT (( #18290 ) ) ;
#12674 = ORIENTED_EDGE ( 'NONE', *, *, #1897, .T. ) ;
#12675 = CONICAL_SURFACE ( 'NONE', #7208, 2.055000000000001492, 0.7853981633974633780 ) ;
#12676 = DIRECTION ( 'NONE',  ( 0.9510565162951534202, 0.3090169943749478398, 0.000000000000000000 ) ) ;
#12677 = MANIFOLD_SOLID_BREP ( 'M5 Clearance Hole1', #4837 ) ;
#12678 = DIRECTION ( 'NONE',  ( -0.000000000000000000, -0.000000000000000000, -1.000000000000000000 ) ) ;
#12679 = DIRECTION ( 'NONE',  ( 0.000000000000000000, 0.000000000000000000, 1.000000000000000000 ) ) ;
#12680 = CARTESIAN_POINT ( 'NONE',  ( 5.200000000000002842, 3.061616997868383634E-16, -2.500000000000000444 ) ) ;
#12682 = CIRCLE ( 'NONE', #11118, 20.30000000000000071 ) ;
#12681 = FACE_BOUND ( 'NONE', #2735, .T. ) ;
#12683 = FACE_OUTER_BOUND ( 'NONE', #19281, .T. ) ;
#12684 = CIRCLE ( 'NONE', #19550, 2.055000000000000160 ) ;
#12685 = EDGE_CURVE ( 'NONE', #2118, #20062, #997, .T. ) ;
#12686 = CARTESIAN_POINT ( 'NONE',  ( 24.99999999999999645, 2.463415629691065208E-15, 145.0000059999999849 ) ) ;
#12687 = AXIS2_PLACEMENT_3D ( 'NONE', #18152, #6916, #7259 ) ;
#12688 = ORIENTED_EDGE ( 'NONE', *, *, #16074, .F. ) ;
#12689 = EDGE_CURVE ( 'NONE', #19505, #22159, #21987, .T. ) ;
#12690 = ORIENTED_EDGE ( 'NONE', *, *, #21075, .T. ) ;
#12691 = CARTESIAN_POINT ( 'NONE',  ( -2.700000000000001510, 0.000000000000000000, -24.69999999999999929 ) ) ;
#12692 = CARTESIAN_POINT ( 'NONE',  ( -45.24999999999994316, 100.0000000000000000, -145.0000000000000284 ) ) ;
#12693 = EDGE_LOOP ( 'NONE', ( #15607, #10110, #16096, #6462 ) ) ;
#12694 = EDGE_CURVE ( 'NONE', #19415, #17134, #21232, .T. ) ;
#12695 = DIRECTION ( 'NONE',  ( -1.000000000000000000, 1.408839003528726857E-14, 6.982962677686266711E-15 ) ) ;
#12696 = DIRECTION ( 'NONE',  ( 1.000000000000000000, 0.000000000000000000, 0.000000000000000000 ) ) ;
#12697 = AXIS2_PLACEMENT_3D ( 'NONE', #13756, #19372, #21078 ) ;
#12698 = EDGE_LOOP ( 'NONE', ( #6412, #582, #18107, #1738 ) ) ;
#12699 = DIRECTION ( 'NONE',  ( 3.736327486719275871E-16, -1.000000000000000000, 3.469446951953613794E-15 ) ) ;
#12700 = DIRECTION ( 'NONE',  ( 5.551115123125785858E-15, 0.000000000000000000, -1.000000000000000000 ) ) ;
#12701 = ORIENTED_EDGE ( 'NONE', *, *, #11541, .T. ) ;
#12702 = AXIS2_PLACEMENT_3D ( 'NONE', #4798, #6979, #19514 ) ;
#12703 = VECTOR ( 'NONE', #19867, 1000.000000000000114 ) ;
#12704 = LINE ( 'NONE', #10996, #10250 ) ;
#12705 = EDGE_CURVE ( 'NONE', #9872, #7615, #7975, .T. ) ;
#12706 = CIRCLE ( 'NONE', #6111, 5.249999999999962697 ) ;
#12707 = ORIENTED_EDGE ( 'NONE', *, *, #14734, .T. ) ;
#12708 = CARTESIAN_POINT ( 'NONE',  ( 119.9257125005557327, -1087.686723660050802, -32.49999999999356959 ) ) ;
#12709 = DIRECTION ( 'NONE',  ( -0.000000000000000000, 1.000000000000000000, -3.469446951953613794E-15 ) ) ;
#12710 = PLANE ( 'NONE',  #20569 ) ;
#12711 = ORIENTED_EDGE ( 'NONE', *, *, #22169, .F. ) ;
#12712 = EDGE_LOOP ( 'NONE', ( #3927, #15665, #10665 ) ) ;
#12713 = DIRECTION ( 'NONE',  ( 0.000000000000000000, 0.000000000000000000, 1.000000000000000000 ) ) ;
#12714 = CARTESIAN_POINT ( 'NONE',  ( -127.4426065742854064, 88.22361005463105244, -27.62591505085368482 ) ) ;
#12715 = PLANE ( 'NONE',  #14241 ) ;
#12716 = DIRECTION ( 'NONE',  ( -0.8191520442889875797, 1.003171929053519570E-16, 0.5735764363510522656 ) ) ;
#12717 = AXIS2_PLACEMENT_3D ( 'NONE', #6367, #18925, #6009 ) ;
#12718 = ORIENTED_EDGE ( 'NONE', *, *, #7978, .T. ) ;
#12719 = CIRCLE ( 'NONE', #6122, 2.649999999999971934 ) ;
#12720 = CARTESIAN_POINT ( 'NONE',  ( 15.24974479720506970, -19.87769063953885507, 145.0000119999999413 ) ) ;
#12721 = CONICAL_SURFACE ( 'NONE', #17664, 4.174999999999999822, 0.9599310885968795892 ) ;
#12722 = CIRCLE ( 'NONE', #2248, 4.000000000000000000 ) ;
#12723 = ADVANCED_FACE ( 'NONE', ( #1043 ), #13325, .F. ) ;
#12724 = EDGE_CURVE ( 'NONE', #12471, #6599, #11644, .T. ) ;
#12725 = VECTOR ( 'NONE', #8658, 1000.000000000000000 ) ;
#12726 = CARTESIAN_POINT ( 'NONE',  ( -285.2000000000014666, -127.0000000000000568, 146.4928932188134638 ) ) ;
#12727 = CARTESIAN_POINT ( 'NONE',  ( 282.1999999999999318, 267.7999999999999545, -146.4928932188133786 ) ) ;
#12728 = ORIENTED_EDGE ( 'NONE', *, *, #11312, .F. ) ;
#12729 = CARTESIAN_POINT ( 'NONE',  ( 1.060314165522845187, 8.048081368953960535, -7.659344964963204383 ) ) ;
#12730 = EDGE_CURVE ( 'NONE', #5160, #22988, #11503, .T. ) ;
#12731 = EDGE_CURVE ( 'NONE', #10287, #1156, #15355, .T. ) ;
#12732 = ORIENTED_EDGE ( 'NONE', *, *, #22339, .T. ) ;
#12733 = PRODUCT ( 'socket head cap screw_iso_ISO 4762 M5 x 25 - 25N', 'socket head cap screw_iso_ISO 4762 M5 x 25 - 25N', '', ( #15100 ) ) ;
#12734 = VECTOR ( 'NONE', #18265, 1000.000000000000000 ) ;
#12735 = CIRCLE ( 'NONE', #18838, 2.499999999999998668 ) ;
#12736 = CIRCLE ( 'NONE', #3859, 145.0000000000000284 ) ;
#12738 = CARTESIAN_POINT ( 'NONE',  ( 34.75000000000005684, 100.0000000000000000, 150.2000000000009550 ) ) ;
#12737 = AXIS2_PLACEMENT_3D ( 'NONE', #20840, #1991, #19006 ) ;
#12739 = AXIS2_PLACEMENT_3D ( 'NONE', #20873, #19039, #2504 ) ;
#12740 = ORIENTED_EDGE ( 'NONE', *, *, #10974, .T. ) ;
#12741 = VECTOR ( 'NONE', #19952, 1000.000000000000000 ) ;
#12742 = VECTOR ( 'NONE', #20974, 1000.000000000000000 ) ;
#12743 = EDGE_CURVE ( 'NONE', #21577, #3347, #23667, .T. ) ;
#12744 = LINE ( 'NONE', #23564, #19654 ) ;
#12745 = CARTESIAN_POINT ( 'NONE',  ( -16.52066876451826616, -1018.834670294809257, 145.0000119999999981 ) ) ;
#12746 = CARTESIAN_POINT ( 'NONE',  ( 10.00000000000000178, 0.000000000000000000, 0.000000000000000000 ) ) ;
#12747 = CARTESIAN_POINT ( 'NONE',  ( -2.500000000000000888, 0.000000000000000000, -4.974599999999998801 ) ) ;
#12748 = AXIS2_PLACEMENT_3D ( 'NONE', #13120, #9459, #15020 ) ;
#12749 = CARTESIAN_POINT ( 'NONE',  ( -281.4928932188135491, -132.2000000000000455, 177.2000000000014097 ) ) ;
#12750 = ORIENTED_EDGE ( 'NONE', *, *, #15108, .T. ) ;
#12751 = DIRECTION ( 'NONE',  ( 0.000000000000000000, 0.4999999999999989453, -0.8660254037844393737 ) ) ;
#12752 = FILL_AREA_STYLE ('',( #16569 ) ) ;
#12754 = ORIENTED_EDGE ( 'NONE', *, *, #5772, .T. ) ;
#12753 = ORIENTED_EDGE ( 'NONE', *, *, #9584, .T. ) ;
#12755 = CARTESIAN_POINT ( 'NONE',  ( -277.2000000000006708, 90.00000000000098055, -35.00000000000001421 ) ) ;
#12757 = AXIS2_PLACEMENT_3D ( 'NONE', #10332, #6449, #2038 ) ;
#12756 = AXIS2_PLACEMENT_3D ( 'NONE', #2448, #985, #17317 ) ;
#12758 = CARTESIAN_POINT ( 'NONE',  ( -25.00000000000000000, 1.865214261513747767E-15, 145.0000119999999697 ) ) ;
#12759 = DIRECTION ( 'NONE',  ( -6.753181414994864868E-15, 6.753181414994864868E-15, -1.000000000000000000 ) ) ;
#12760 = VECTOR ( 'NONE', #15060, 1000.000000000000114 ) ;
#12761 = CONICAL_SURFACE ( 'NONE', #17734, 2.055000000000001492, 0.7853981633974633780 ) ;
#12762 = EDGE_LOOP ( 'NONE', ( #804, #5495 ) ) ;
#12763 = CARTESIAN_POINT ( 'NONE',  ( 107.6499999999999631, 35.00000000000000000, 3.000000000000000000 ) ) ;
#12764 = EDGE_CURVE ( 'NONE', #14056, #18892, #20195, .T. ) ;
#12765 = EDGE_CURVE ( 'NONE', #16072, #9980, #12331, .T. ) ;
#12766 = FACE_OUTER_BOUND ( 'NONE', #4398, .T. ) ;
#12767 = ADVANCED_FACE ( 'NONE', ( #6486 ), #21456, .F. ) ;
#12768 = ORIENTED_EDGE ( 'NONE', *, *, #9100, .F. ) ;
#12769 = EDGE_CURVE ( 'NONE', #12500, #22877, #15463, .T. ) ;
#12770 = DIRECTION ( 'NONE',  ( -1.000000000000000000, 0.000000000000000000, 0.000000000000000000 ) ) ;
#12771 =( NAMED_UNIT ( * ) SI_UNIT ( $, .STERADIAN. ) SOLID_ANGLE_UNIT ( ) );
#12772 = CONTEXT_DEPENDENT_SHAPE_REPRESENTATION ( #20188, #17577 ) ;
#12773 = VERTEX_POINT ( 'NONE', #6976 ) ;
#12774 = VERTEX_POINT ( 'NONE', #18194 ) ;
#12775 = EDGE_CURVE ( 'NONE', #14717, #1127, #21743, .T. ) ;
#12776 = CARTESIAN_POINT ( 'NONE',  ( 125.3835310783086356, -1091.126227143374535, 28.00959664470840238 ) ) ;
#12777 = AXIS2_PLACEMENT_3D ( 'NONE', #9839, #17537, #767 ) ;
#12778 = EDGE_LOOP ( 'NONE', ( #21706, #15726, #4697, #11038 ) ) ;
#12779 = EDGE_CURVE ( 'NONE', #16229, #7198, #1299, .T. ) ;
#12780 = CARTESIAN_POINT ( 'NONE',  ( -129.3177328886530120, 85.45129583908924076, 30.16873261443288001 ) ) ;
#12781 = MECHANICAL_DESIGN_GEOMETRIC_PRESENTATION_REPRESENTATION (  '', ( #14675 ), #20420 ) ;
#12782 = AXIS2_PLACEMENT_3D ( 'NONE', #3622, #21998, #17903 ) ;
#12783 = CARTESIAN_POINT ( 'NONE',  ( 133.8639378433819047, 78.13740870752447165, 31.53022738271491576 ) ) ;
#12784 = VECTOR ( 'NONE', #3504, 1000.000000000000000 ) ;
#12785 = CONICAL_SURFACE ( 'NONE', #13178, 2.055000000000001492, 0.7853981633974633780 ) ;
#12786 = LINE ( 'NONE', #16466, #3401 ) ;
#12787 = LINE ( 'NONE', #8762, #13705 ) ;
#12788 = DIRECTION ( 'NONE',  ( -1.000000000000000000, 1.408839003528726857E-14, 6.982962677686266711E-15 ) ) ;
#12789 = ITEM_DEFINED_TRANSFORMATION ( 'NONE', 'NONE', #17725,  #11210 ) ;
#12790 = AXIS2_PLACEMENT_3D ( 'NONE', #11470, #2252, #467 ) ;
#12791 = ORIENTED_EDGE ( 'NONE', *, *, #10549, .F. ) ;
#12792 = DIRECTION ( 'NONE',  ( -1.000000000000000000, 1.408839003528726857E-14, 0.000000000000000000 ) ) ;
#12793 = CARTESIAN_POINT ( 'NONE',  ( -7.499999999999998224, 1.489914625143999416, -0.1187923833806747292 ) ) ;
#12794 = CARTESIAN_POINT ( 'NONE',  ( -0.6640947660597427138, 4.471078309994878985, -3.602146406945963442 ) ) ;
#12795 = ORIENTED_EDGE ( 'NONE', *, *, #10933, .T. ) ;
#12796 = DIRECTION ( 'NONE',  ( 0.000000000000000000, -1.000000000000000000, 0.000000000000000000 ) ) ;
#12797 = CARTESIAN_POINT ( 'NONE',  ( -7.500000000000000000, -4.330127018922198090, -10.00000000000000000 ) ) ;
#12798 = AXIS2_PLACEMENT_3D ( 'NONE', #5459, #5338, #21866 ) ;
#12799 = CIRCLE ( 'NONE', #15851, 2.499999999999998668 ) ;
#12800 = CARTESIAN_POINT ( 'NONE',  ( -280.5758453455904942, 269.9427398886703031, 145.2488155364689248 ) ) ;
#12801 = VECTOR ( 'NONE', #19344, 1000.000000000000000 ) ;
#12802 = DIRECTION ( 'NONE',  ( 0.000000000000000000, 0.000000000000000000, -1.000000000000000000 ) ) ;
#12803 = CARTESIAN_POINT ( 'NONE',  ( 146.4449999999997942, -209.9999999999996874, 27.50000000000642331 ) ) ;
#12804 = ORIENTED_EDGE ( 'NONE', *, *, #4255, .T. ) ;
#12805 = CARTESIAN_POINT ( 'NONE',  ( -2.700000000000001066, 0.000000000000000000, 0.000000000000000000 ) ) ;
#12806 = EDGE_LOOP ( 'NONE', ( #8373, #17453, #20650, #5117 ) ) ;
#12807 = CARTESIAN_POINT ( 'NONE',  ( -282.2000000000014666, -127.0000000000000568, 146.4928932188134638 ) ) ;
#12808 = ADVANCED_FACE ( 'NONE', ( #1406 ), #10505, .T. ) ;
#12809 = ADVANCED_FACE ( 'NONE', ( #16382 ), #9022, .F. ) ;
#12810 = ORIENTED_EDGE ( 'NONE', *, *, #179, .F. ) ;
#12811 = CARTESIAN_POINT ( 'NONE',  ( 7.499999999999997335, 34.18698582794336005, 100.0000000000000000 ) ) ;
#12812 = CARTESIAN_POINT ( 'NONE',  ( 123.7129353098586932, -1093.381627813014120, -27.82770220384456650 ) ) ;
#12813 = CARTESIAN_POINT ( 'NONE',  ( -79.99999999999995737, -59.80000000000003268, 5.199999999999982414 ) ) ;
#12814 = CARTESIAN_POINT ( 'NONE',  ( 0.000000000000000000, 0.000000000000000000, 3.469446951953614189E-15 ) ) ;
#12815 = DIRECTION ( 'NONE',  ( -1.000000000000000000, -0.000000000000000000, -0.000000000000000000 ) ) ;
#12816 = DIRECTION ( 'NONE',  ( 1.000000000000000000, 0.000000000000000000, 0.000000000000000000 ) ) ;
#12817 = CARTESIAN_POINT ( 'NONE',  ( -21.69578997558840427, 12.52876685377503208, 145.0000119999999697 ) ) ;
#12818 = VERTEX_POINT ( 'NONE', #23733 ) ;
#12819 = VERTEX_POINT ( 'NONE', #7188 ) ;
#12820 = FACE_OUTER_BOUND ( 'NONE', #5822, .T. ) ;
#12821 = PLANE ( 'NONE',  #15041 ) ;
#12822 = VERTEX_POINT ( 'NONE', #18296 ) ;
#12823 = CARTESIAN_POINT ( 'NONE',  ( 119.6158142514527469, -1087.367367941136308, 27.94500000000641293 ) ) ;
#12824 = CARTESIAN_POINT ( 'NONE',  ( -194.7500000000000284, -784.4690652294799520, 30.00000000000675726 ) ) ;
#12825 = VERTEX_POINT ( 'NONE', #12680 ) ;
#12826 = DIRECTION ( 'NONE',  ( -1.000000000000000000, -0.000000000000000000, -0.000000000000000000 ) ) ;
#12827 = DIRECTION ( 'NONE',  ( 0.8660254037844382635, 0.5000000000000004441, 0.000000000000000000 ) ) ;
#12828 = ORIENTED_EDGE ( 'NONE', *, *, #647, .T. ) ;
#12829 = DIRECTION ( 'NONE',  ( -0.000000000000000000, 0.000000000000000000, 1.000000000000000000 ) ) ;
#12830 = FACE_OUTER_BOUND ( 'NONE', #13683, .T. ) ;
#12831 = VERTEX_POINT ( 'NONE', #5053 ) ;
#12832 = CARTESIAN_POINT ( 'NONE',  ( -194.7500000000004547, -784.4690652294792699, -27.49999999999322498 ) ) ;
#12833 = CARTESIAN_POINT ( 'NONE',  ( -136.5243927815876361, -1073.390114808524004, 31.99235058689517430 ) ) ;
#12834 = CARTESIAN_POINT ( 'NONE',  ( -4.211140560182196957, 2.431303136016537803, -3.745885042887433514 ) ) ;
#12835 = ORIENTED_EDGE ( 'NONE', *, *, #15383, .T. ) ;
#12836 = EDGE_LOOP ( 'NONE', ( #5481, #4522, #14606, #20538 ) ) ;
#12837 = DIRECTION ( 'NONE',  ( -1.000000000000000000, 1.408839003528726857E-14, 6.982962677686266711E-15 ) ) ;
#12838 = PRODUCT_DEFINITION_SHAPE ( 'NONE', 'NONE',  #23887 ) ;
#12839 = APPLICATION_PROTOCOL_DEFINITION ( 'draft international standard', 'automotive_design', 1998, #13590 ) ;
#12840 = DIRECTION ( 'NONE',  ( 1.000000000000000000, 0.000000000000000000, -0.000000000000000000 ) ) ;
#12841 = CARTESIAN_POINT ( 'NONE',  ( 34.75000000000005684, 100.0000000000000000, -125.0000000000000000 ) ) ;
#12842 = DIRECTION ( 'NONE',  ( -0.000000000000000000, 1.000000000000000000, -3.469446951953613794E-15 ) ) ;
#12843 = ORIENTED_EDGE ( 'NONE', *, *, #6648, .T. ) ;
#12844 = LINE ( 'NONE', #11129, #16854 ) ;
#12845 = UNCERTAINTY_MEASURE_WITH_UNIT (LENGTH_MEASURE( 1.000000000000000082E-05 ), #17994, 'distance_accuracy_value', 'NONE');
#12846 = CARTESIAN_POINT ( 'NONE',  ( 25.00000000000001066, 45.00100000000033162, 34.99999999999983658 ) ) ;
#12847 = DIRECTION ( 'NONE',  ( 0.000000000000000000, 2.618450529776313049E-15, 1.000000000000000000 ) ) ;
#12848 = ORIENTED_EDGE ( 'NONE', *, *, #14524, .F. ) ;
#12849 =( REPRESENTATION_RELATIONSHIP ('NONE','NONE', #10127, #8987 ) REPRESENTATION_RELATIONSHIP_WITH_TRANSFORMATION ( #23588 )SHAPE_REPRESENTATION_RELATIONSHIP( ) );
#12850 = DIRECTION ( 'NONE',  ( 0.000000000000000000, 0.000000000000000000, 1.000000000000000000 ) ) ;
#12851 = ORIENTED_EDGE ( 'NONE', *, *, #16367, .F. ) ;
#12852 = CARTESIAN_POINT ( 'NONE',  ( 5.000000000000015099, 0.000000000000000000, 4.250000000000000000 ) ) ;
#12853 = CARTESIAN_POINT ( 'NONE',  ( -35.00000000000001421, 90.00000000000001421, 3.000000000000001332 ) ) ;
#12854 = ORIENTED_EDGE ( 'NONE', *, *, #16972, .T. ) ;
#12855 = EDGE_CURVE ( 'NONE', #3554, #11487, #8664, .T. ) ;
#12856 = CARTESIAN_POINT ( 'NONE',  ( -287.4000000000014552, -132.2000000000000455, -146.4928932188134070 ) ) ;
#12857 = CARTESIAN_POINT ( 'NONE',  ( 12.52876685377503208, -1021.695789975588241, 145.0000119999999697 ) ) ;
#12858 = EDGE_CURVE ( 'NONE', #3485, #7620, #12536, .T. ) ;
#12859 = EDGE_CURVE ( 'NONE', #18998, #1257, #2464, .T. ) ;
#12860 = CYLINDRICAL_SURFACE ( 'NONE', #314, 2.500000000000002220 ) ;
#12861 = CARTESIAN_POINT ( 'NONE',  ( 124.8644691973859295, -1091.836575763270957, -32.43450926607476248 ) ) ;
#12862 = FACE_OUTER_BOUND ( 'NONE', #5221, .T. ) ;
#12863 = EDGE_LOOP ( 'NONE', ( #17685, #20891, #14036 ) ) ;
#12864 = DIRECTION ( 'NONE',  ( -0.000000000000000000, 3.483493295888648978E-15, 1.000000000000000000 ) ) ;
#12865 = ADVANCED_FACE ( 'NONE', ( #16037 ), #6845, .F. ) ;
#12866 = CIRCLE ( 'NONE', #21683, 2.055000000000001492 ) ;
#12868 = ORIENTED_EDGE ( 'NONE', *, *, #15548, .F. ) ;
#12867 = ORIENTED_EDGE ( 'NONE', *, *, #580, .F. ) ;
#12869 = CARTESIAN_POINT ( 'NONE',  ( -293.2000000000010118, 90.00000000000029843, -34.99999999999928235 ) ) ;
#12870 = DIRECTION ( 'NONE',  ( -0.000000000000000000, 1.000000000000000000, -3.469446951953613794E-15 ) ) ;
#12871 = FACE_OUTER_BOUND ( 'NONE', #9777, .T. ) ;
#12872 = ORIENTED_EDGE ( 'NONE', *, *, #20465, .T. ) ;
#12873 = DIRECTION ( 'NONE',  ( -1.000000000000000000, -0.000000000000000000, -0.000000000000000000 ) ) ;
#12874 = CARTESIAN_POINT ( 'NONE',  ( 119.6158142514525764, -1087.367367941136990, -32.05499999999357641 ) ) ;
#12875 = ORIENTED_EDGE ( 'NONE', *, *, #9719, .T. ) ;
#12876 = CARTESIAN_POINT ( 'NONE',  ( 0.2500000000000002220, 5.204748896376250699E-16, -4.250000000000000000 ) ) ;
#12877 = FACE_OUTER_BOUND ( 'NONE', #11932, .T. ) ;
#12878 = ITEM_DEFINED_TRANSFORMATION ( 'NONE', 'NONE', #17379,  #11210 ) ;
#12879 = VERTEX_POINT ( 'NONE', #9139 ) ;
#12880 = AXIS2_PLACEMENT_3D ( 'NONE', #17129, #6263, #15213 ) ;
#12881 = ORIENTED_EDGE ( 'NONE', *, *, #11998, .F. ) ;
#12882 = CARTESIAN_POINT ( 'NONE',  ( 125.9653219304451000, -1090.320195256218767, 29.67150201188739089 ) ) ;
#12883 = ORIENTED_EDGE ( 'NONE', *, *, #9935, .F. ) ;
#12884 = CARTESIAN_POINT ( 'NONE',  ( 15.25457574328937227, -980.1254780500729566, -145.0000000000001137 ) ) ;
#12885 = CARTESIAN_POINT ( 'NONE',  ( 132.8404720734530144, 79.86494211668951948, 32.50000000000646594 ) ) ;
#12886 = CARTESIAN_POINT ( 'NONE',  ( -85.22886158240795851, -117.3074641843678876, -90.00000000000000000 ) ) ;
#12887 = EDGE_CURVE ( 'NONE', #711, #3985, #12928, .T. ) ;
#12888 = CYLINDRICAL_SURFACE ( 'NONE', #10604, 5.199999999999982414 ) ;
#12889 = DIRECTION ( 'NONE',  ( 0.000000000000000000, 0.000000000000000000, -1.000000000000000000 ) ) ;
#12890 = EDGE_CURVE ( 'NONE', #18256, #17025, #5154, .T. ) ;
#12891 = ADVANCED_FACE ( 'NONE', ( #12459 ), #12151, .F. ) ;
#12892 = ORIENTED_EDGE ( 'NONE', *, *, #16478, .T. ) ;
#12893 = VECTOR ( 'NONE', #18378, 999.9999999999998863 ) ;
#12894 = CARTESIAN_POINT ( 'NONE',  ( 162.9999999999998010, -499.9999999999996589, 30.00000000000653699 ) ) ;
#12895 = CARTESIAN_POINT ( 'NONE',  ( 105.0000000000000000, -19.99999999999998934, 0.000000000000000000 ) ) ;
#12896 = DIRECTION ( 'NONE',  ( -0.9289202219288174023, -0.3702799228849933955, -6.982962677686267499E-15 ) ) ;
#12897 = CIRCLE ( 'NONE', #9385, 1.499999999999999556 ) ;
#12898 = EDGE_LOOP ( 'NONE', ( #19320, #1712 ) ) ;
#12899 = EDGE_CURVE ( 'NONE', #21466, #18256, #12567, .T. ) ;
#12900 = CARTESIAN_POINT ( 'NONE',  ( 2.500000000000000000, -2.357898499370432610, 3.252606517456513302E-15 ) ) ;
#12901 = FACE_OUTER_BOUND ( 'NONE', #19548, .T. ) ;
#12902 = CARTESIAN_POINT ( 'NONE',  ( -282.2000000000000455, 268.0880230824753312, 146.3684665479255500 ) ) ;
#12903 = DIRECTION ( 'NONE',  ( 0.000000000000000000, 0.000000000000000000, -1.000000000000000000 ) ) ;
#12904 = DIRECTION ( 'NONE',  ( -6.640089860198304064E-16, -1.000000000000000000, 3.495664435217746987E-15 ) ) ;
#12905 = ORIENTED_EDGE ( 'NONE', *, *, #7743, .T. ) ;
#12907 = CARTESIAN_POINT ( 'NONE',  ( -281.4928932188135491, -132.2000000000000455, 152.4000000000014268 ) ) ;
#12906 = VECTOR ( 'NONE', #5180, 1000.000000000000000 ) ;
#12908 = ORIENTED_EDGE ( 'NONE', *, *, #3731, .T. ) ;
#12909 = DIRECTION ( 'NONE',  ( 1.000000000000000000, 0.000000000000000000, 0.000000000000000000 ) ) ;
#12910 = VECTOR ( 'NONE', #19758, 1000.000000000000000 ) ;
#12911 = CARTESIAN_POINT ( 'NONE',  ( -110.0000000000000142, 95.00000000000001421, 3.000000000000000000 ) ) ;
#12912 = ORIENTED_EDGE ( 'NONE', *, *, #5286, .T. ) ;
#12913 = CARTESIAN_POINT ( 'NONE',  ( 123.5484583266983094, -1093.599130927305623, -31.99339931332756493 ) ) ;
#12914 = CARTESIAN_POINT ( 'NONE',  ( -288.2000000000008981, 30.00000000000101963, -105.0000000000000142 ) ) ;
#12915 = DIRECTION ( 'NONE',  ( 1.000000000000000000, 0.000000000000000000, 0.000000000000000000 ) ) ;
#12916 = CARTESIAN_POINT ( 'NONE',  ( -122.8605704798722940, 82.74225173005859801, 32.05500000000641592 ) ) ;
#12917 = CARTESIAN_POINT ( 'NONE',  ( 1.500000000000000000, 9.886859966642592923, -50.00000000000000000 ) ) ;
#12918 = DIRECTION ( 'NONE',  ( -0.9423651898111409242, -0.3345860861306287903, 6.982962677686267499E-15 ) ) ;
#12919 = ORIENTED_EDGE ( 'NONE', *, *, #8132, .F. ) ;
#12920 = ORIENTED_EDGE ( 'NONE', *, *, #10932, .T. ) ;
#12921 = DIRECTION ( 'NONE',  ( -1.000000000000000000, -0.000000000000000000, -0.000000000000000000 ) ) ;
#12922 = DIRECTION ( 'NONE',  ( 1.000000000000000000, -0.000000000000000000, 6.982962677686266711E-15 ) ) ;
#12923 = ORIENTED_EDGE ( 'NONE', *, *, #10151, .F. ) ;
#12924 = MECHANICAL_DESIGN_GEOMETRIC_PRESENTATION_REPRESENTATION (  '', ( #20193 ), #15227 ) ;
#12925 = PRODUCT ( 'driver shaft', 'driver shaft', '', ( #21230 ) ) ;
#12926 = CARTESIAN_POINT ( 'NONE',  ( 281.4928932188133217, -127.0000000000000568, 152.4000000000014268 ) ) ;
#12928 = CIRCLE ( 'NONE', #2059, 2.500000000000000888 ) ;
#12927 = CARTESIAN_POINT ( 'NONE',  ( 1.249327701954825010, -8.410337540182549532, -7.776713651265369620 ) ) ;
#12929 = ADVANCED_FACE ( 'NONE', ( #19878, #1532, #8922, #16280, #14466 ), #21807, .F. ) ;
#12930 = ADVANCED_FACE ( 'NONE', ( #22274 ), #7798, .F. ) ;
#12931 = EDGE_CURVE ( 'NONE', #506, #16172, #20470, .T. ) ;
#12932 = CIRCLE ( 'NONE', #22183, 7.500000000000000000 ) ;
#12933 = VERTEX_POINT ( 'NONE', #9500 ) ;
#12934 = CARTESIAN_POINT ( 'NONE',  ( 280.9952621458755289, 270.4188186979286002, 149.5436892194421716 ) ) ;
#12935 = CARTESIAN_POINT ( 'NONE',  ( -10.00000000000000000, 1.183534169888512011, 200.0000120000000265 ) ) ;
#12936 = ORIENTED_EDGE ( 'NONE', *, *, #11700, .T. ) ;
#12937 = CARTESIAN_POINT ( 'NONE',  ( 0.000000000000000000, 0.000000000000000000, 0.000000000000000000 ) ) ;
#12938 = DIRECTION ( 'NONE',  ( 0.000000000000000000, -3.469446951953614583E-15, -1.000000000000000000 ) ) ;
#12939 = CARTESIAN_POINT ( 'NONE',  ( -9.999999999999998224, -6.123233995736763324E-16, 200.0000060000000133 ) ) ;
#12940 = VERTEX_POINT ( 'NONE', #1869 ) ;
#12941 = CARTESIAN_POINT ( 'NONE',  ( 7.500000000000000000, 4.330127018922190096, -7.422398894150032511 ) ) ;
#12942 = DIRECTION ( 'NONE',  ( 0.000000000000000000, 0.000000000000000000, -1.000000000000000000 ) ) ;
#12943 = VERTEX_POINT ( 'NONE', #5625 ) ;
#12944 = ORIENTED_EDGE ( 'NONE', *, *, #4891, .T. ) ;
#12945 = CARTESIAN_POINT ( 'NONE',  ( 7.922281120364393914, 4.573931137438269623, -8.047472243342930653 ) ) ;
#12946 = AXIS2_PLACEMENT_3D ( 'NONE', #16625, #4157, #20699 ) ;
#12947 = SHAPE_DEFINITION_REPRESENTATION ( #17677, #15622 ) ;
#12948 = CARTESIAN_POINT ( 'NONE',  ( 0.000000000000000000, 0.000000000000000000, 0.000000000000000000 ) ) ;
#12949 = AXIS2_PLACEMENT_3D ( 'NONE', #7638, #15032, #11189 ) ;
#12950 = FACE_OUTER_BOUND ( 'NONE', #4221, .T. ) ;
#12951 = CARTESIAN_POINT ( 'NONE',  ( -158.1195828810603246, 116.4077317428679805, 32.50000000000675726 ) ) ;
#12952 = AXIS2_PLACEMENT_3D ( 'NONE', #20595, #14836, #4312 ) ;
#12953 = VERTEX_POINT ( 'NONE', #20580 ) ;
#12954 = CARTESIAN_POINT ( 'NONE',  ( 232.0000000000000568, -557.0000000000000000, -57.00000000000000000 ) ) ;
#12955 = EDGE_CURVE ( 'NONE', #8474, #10308, #7917, .T. ) ;
#12956 = PRODUCT_DEFINITION_CONTEXT ( 'detailed design', #11742, 'design' ) ;
#12957 = VERTEX_POINT ( 'NONE', #16991 ) ;
#12958 = CARTESIAN_POINT ( 'NONE',  ( 281.4928932188133217, -129.2000000000000455, 152.4000000000014268 ) ) ;
#12959 = ADVANCED_FACE ( 'NONE', ( #83 ), #3919, .F. ) ;
#12960 = CARTESIAN_POINT ( 'NONE',  ( 146.0000000000002274, -801.0618695410406644, -29.99999999999356604 ) ) ;
#12961 = ORIENTED_EDGE ( 'NONE', *, *, #5330, .F. ) ;
#12962 = CARTESIAN_POINT ( 'NONE',  ( 0.000000000000000000, 0.000000000000000000, 100.0000000000000000 ) ) ;
#12963 = CIRCLE ( 'NONE', #19079, 5.249999999999949374 ) ;
#12964 = ORIENTED_EDGE ( 'NONE', *, *, #17698, .T. ) ;
#12965 = CARTESIAN_POINT ( 'NONE',  ( -285.2000000000012960, -74.99999999999899103, -90.00000000000000000 ) ) ;
#12966 = DIRECTION ( 'NONE',  ( -0.7071067811865369146, 8.659560562355062281E-17, -0.7071067811865582309 ) ) ;
#12967 = ORIENTED_EDGE ( 'NONE', *, *, #20975, .T. ) ;
#12968 = LINE ( 'NONE', #12528, #20029 ) ;
#12969 = FACE_OUTER_BOUND ( 'NONE', #20869, .T. ) ;
#12970 = CIRCLE ( 'NONE', #11820, 2.055000000000001492 ) ;
#12971 = CARTESIAN_POINT ( 'NONE',  ( 282.3062614524587275, 272.4728700860326853, 145.4358181722191432 ) ) ;
#12972 = APPLICATION_CONTEXT ( 'automotive_design' ) ;
#12973 = CARTESIAN_POINT ( 'NONE',  ( 125.9653219304447447, -1090.320195256219449, -30.32849798811274411 ) ) ;
#12974 = LINE ( 'NONE', #5682, #17708 ) ;
#12975 = ORIENTED_EDGE ( 'NONE', *, *, #84, .F. ) ;
#12976 = CARTESIAN_POINT ( 'NONE',  ( 155.0000000000000284, -500.0000000000000000, 27.35000000000002629 ) ) ;
#12977 = DIRECTION ( 'NONE',  ( 0.000000000000000000, -1.000000000000000000, 0.000000000000000000 ) ) ;
#12978 = EDGE_CURVE ( 'NONE', #22845, #13209, #20969, .T. ) ;
#12979 = AXIS2_PLACEMENT_3D ( 'NONE', #22204, #2403, #20396 ) ;
#12981 = VERTEX_POINT ( 'NONE', #20336 ) ;
#12980 = VERTEX_POINT ( 'NONE', #7552 ) ;
#12982 = TOROIDAL_SURFACE ( 'NONE', #3243, 10.12668159690567649, 0.7733184030943209830 ) ;
#12983 = DIRECTION ( 'NONE',  ( 0.9237280213470682178, 0.3830490080632377725, 1.131240564625405124E-16 ) ) ;
#12984 = CARTESIAN_POINT ( 'NONE',  ( -135.9481979339309135, -1074.452087582500099, -32.48402282453943002 ) ) ;
#12985 = CARTESIAN_POINT ( 'NONE',  ( 281.4928932188134354, 267.8000000000000114, -147.1696999999999207 ) ) ;
#12986 = ORIENTED_EDGE ( 'NONE', *, *, #912, .F. ) ;
#12987 = ADVANCED_FACE ( 'NONE', ( #18762, #20704 ), #22514, .F. ) ;
#12988 = DIRECTION ( 'NONE',  ( 0.000000000000000000, 0.000000000000000000, -1.000000000000000000 ) ) ;
#12989 = ORIENTED_EDGE ( 'NONE', *, *, #7650, .T. ) ;
#12990 = VECTOR ( 'NONE', #8302, 1000.000000000000114 ) ;
#12991 = EDGE_CURVE ( 'NONE', #14389, #6861, #15600, .T. ) ;
#12992 = CARTESIAN_POINT ( 'NONE',  ( 312.2000000000013529, -132.2000000000000455, -146.4928932188134070 ) ) ;
#12993 = ORIENTED_EDGE ( 'NONE', *, *, #5924, .F. ) ;
#12994 = DIRECTION ( 'NONE',  ( -1.000000000000000000, 0.000000000000000000, -6.982962677686266711E-15 ) ) ;
#12995 = CARTESIAN_POINT ( 'NONE',  ( -129.6400180686265173, -1072.557589128678728, 30.00000000000641975 ) ) ;
#12996 = EDGE_CURVE ( 'NONE', #3977, #2027, #5170, .T. ) ;
#12997 = CONTEXT_DEPENDENT_SHAPE_REPRESENTATION ( #776, #23176 ) ;
#12998 = ORIENTED_EDGE ( 'NONE', *, *, #5892, .T. ) ;
#12999 = CIRCLE ( 'NONE', #4064, 5.200000000000028599 ) ;
#13000 = CARTESIAN_POINT ( 'NONE',  ( 0.000000000000000000, 4.685197434473814759, -5.637851296924623057E-15 ) ) ;
#13001 = ORIENTED_EDGE ( 'NONE', *, *, #2780, .T. ) ;
#13002 = CARTESIAN_POINT ( 'NONE',  ( -280.4358181722192285, 272.4728700860326285, 147.3062614524587275 ) ) ;
#13003 = DIRECTION ( 'NONE',  ( 1.000000000000000000, 0.000000000000000000, 0.000000000000000000 ) ) ;
#13004 = CARTESIAN_POINT ( 'NONE',  ( -282.2000000000006708, 90.00000000000100897, 37.64999999999996305 ) ) ;
#13005 = CARTESIAN_POINT ( 'NONE',  ( 2.999999999999995559, 0.000000000000000000, -21.02499999999999858 ) ) ;
#13006 = FACE_OUTER_BOUND ( 'NONE', #9342, .T. ) ;
#13007 = AXIS2_PLACEMENT_3D ( 'NONE', #23687, #3522, #3282 ) ;
#13008 = ORIENTED_EDGE ( 'NONE', *, *, #15383, .F. ) ;
#13009 = FILL_AREA_STYLE ('',( #16830 ) ) ;
#13010 = CARTESIAN_POINT ( 'NONE',  ( -7.500000000000000888, 2.575910028905295857, -0.3641256808890092067 ) ) ;
#13011 = FACE_OUTER_BOUND ( 'NONE', #11161, .T. ) ;
#13012 = ORIENTED_EDGE ( 'NONE', *, *, #21253, .F. ) ;
#13013 = DIRECTION ( 'NONE',  ( 3.469446951953614682E-16, -1.000000000000000000, 3.483493295888648978E-15 ) ) ;
#13014 = EDGE_CURVE ( 'NONE', #5669, #7880, #14823, .T. ) ;
#13015 = CARTESIAN_POINT ( 'NONE',  ( 1.500000000000000000, 9.886859966642591147, 150.0000000000000284 ) ) ;
#13016 = EDGE_CURVE ( 'NONE', #1301, #14664, #13693, .T. ) ;
#13017 = CARTESIAN_POINT ( 'NONE',  ( 7.500000000000001776, 0.000000000000000000, 0.000000000000000000 ) ) ;
#13018 = AXIS2_PLACEMENT_3D ( 'NONE', #7504, #7991, #22359 ) ;
#13019 = LINE ( 'NONE', #13259, #1325 ) ;
#13020 = CARTESIAN_POINT ( 'NONE',  ( 2.500000000000000000, -1.178949249685214307, 2.042000000000001592 ) ) ;
#13021 = EDGE_CURVE ( 'NONE', #160, #17167, #8510, .T. ) ;
#13022 = VECTOR ( 'NONE', #10477, 1000.000000000000000 ) ;
#13023 = ORIENTED_EDGE ( 'NONE', *, *, #271, .F. ) ;
#13024 = CARTESIAN_POINT ( 'NONE',  ( -24.99999999999998224, -1000.000000000000000, 145.0000059999999280 ) ) ;
#13025 = ADVANCED_FACE ( 'NONE', ( #20224 ), #7676, .F. ) ;
#13026 = VERTEX_POINT ( 'NONE', #22154 ) ;
#13027 = DIRECTION ( 'NONE',  ( 0.000000000000000000, 0.000000000000000000, -1.000000000000000000 ) ) ;
#13028 = DIRECTION ( 'NONE',  ( 0.000000000000000000, 0.000000000000000000, 1.000000000000000000 ) ) ;
#13029 = LINE ( 'NONE', #20331, #15997 ) ;
#13030 = ORIENTED_EDGE ( 'NONE', *, *, #11860, .T. ) ;
#13031 = CARTESIAN_POINT ( 'NONE',  ( 2.500000000000000000, 2.357898499370431722, -2.818925648462311528E-15 ) ) ;
#13032 = EDGE_CURVE ( 'NONE', #23797, #12522, #16630, .T. ) ;
#13033 = CARTESIAN_POINT ( 'NONE',  ( 122.9957307409590186, -1094.324181863848480, -29.34813586885355363 ) ) ;
#13034 = DIRECTION ( 'NONE',  ( 0.000000000000000000, 0.000000000000000000, -1.000000000000000000 ) ) ;
#13035 = CARTESIAN_POINT ( 'NONE',  ( -31.74999999999994316, 0.000000000000000000, 2.500000000000000444 ) ) ;
#13036 = DIRECTION ( 'NONE',  ( 1.000000000000000000, -0.000000000000000000, -0.000000000000000000 ) ) ;
#13037 = EDGE_CURVE ( 'NONE', #14870, #15759, #15070, .T. ) ;
#13038 = LINE ( 'NONE', #12917, #15399 ) ;
#13039 = VECTOR ( 'NONE', #7467, 1000.000000000000000 ) ;
#13040 = CARTESIAN_POINT ( 'NONE',  ( 100.0000000000000000, 249.9999999999999716, 125.0000000000000284 ) ) ;
#13041 = ORIENTED_EDGE ( 'NONE', *, *, #10573, .F. ) ;
#13042 = ORIENTED_EDGE ( 'NONE', *, *, #1430, .T. ) ;
#13043 = FACE_OUTER_BOUND ( 'NONE', #18186, .T. ) ;
#13044 = AXIS2_PLACEMENT_3D ( 'NONE', #15474, #2762, #15827 ) ;
#13045 = DIRECTION ( 'NONE',  ( 0.000000000000000000, 1.000000000000000000, 0.000000000000000000 ) ) ;
#13046 = ORIENTED_EDGE ( 'NONE', *, *, #871, .T. ) ;
#13047 = DIRECTION ( 'NONE',  ( -1.000000000000000000, 0.000000000000000000, 0.000000000000000000 ) ) ;
#13048 = CARTESIAN_POINT ( 'NONE',  ( 6.625705691649528717, -5.306270977113132226, -7.795653906408932521 ) ) ;
#13049 = DIRECTION ( 'NONE',  ( -1.000000000000000000, -0.000000000000000000, -0.000000000000000000 ) ) ;
#13050 = ORIENTED_EDGE ( 'NONE', *, *, #14215, .T. ) ;
#13051 = EDGE_CURVE ( 'NONE', #14252, #20139, #915, .T. ) ;
#13052 = DIRECTION ( 'NONE',  ( -0.000000000000000000, 1.000000000000000000, 0.000000000000000000 ) ) ;
#13053 = FACE_BOUND ( 'NONE', #993, .T. ) ;
#13054 = CARTESIAN_POINT ( 'NONE',  ( 6.145467199749148790, -7.996668423981797780, 200.0000119999999697 ) ) ;
#13055 = ORIENTED_EDGE ( 'NONE', *, *, #22522, .T. ) ;
#13056 = DIRECTION ( 'NONE',  ( -0.000000000000000000, -0.000000000000000000, 1.000000000000000000 ) ) ;
#13057 = DIRECTION ( 'NONE',  ( 1.000000000000000000, 0.000000000000000000, 0.000000000000000000 ) ) ;
#13058 = EDGE_CURVE ( 'NONE', #3015, #19875, #14441, .T. ) ;
#13059 = VECTOR ( 'NONE', #3166, 999.9999999999998863 ) ;
#13060 = CARTESIAN_POINT ( 'NONE',  ( 1.500000000000000000, 9.886859966642592923, 0.000000000000000000 ) ) ;
#13061 = VECTOR ( 'NONE', #9163, 999.9999999999997726 ) ;
#13062 = ORIENTED_EDGE ( 'NONE', *, *, #747, .T. ) ;
#13063 = CARTESIAN_POINT ( 'NONE',  ( 2.500000000000000000, -1.178949249685213863, 2.042000000000001148 ) ) ;
#13064 = APPLICATION_PROTOCOL_DEFINITION ( 'draft international standard', 'automotive_design', 1998, #18458 ) ;
#13065 = FACE_OUTER_BOUND ( 'NONE', #12778, .T. ) ;
#13066 = ADVANCED_FACE ( 'NONE', ( #15769 ), #7094, .T. ) ;
#13067 = EDGE_CURVE ( 'NONE', #2497, #17622, #22526, .T. ) ;
#13068 = EDGE_CURVE ( 'NONE', #22784, #17056, #14088, .T. ) ;
#13069 = LINE ( 'NONE', #15102, #20744 ) ;
#13070 = CARTESIAN_POINT ( 'NONE',  ( 35.00000000000000000, 4.286263797015736496E-15, 100.0000000000000000 ) ) ;
#13071 = VERTEX_POINT ( 'NONE', #15897 ) ;
#13072 = VERTEX_POINT ( 'NONE', #10217 ) ;
#13073 = CARTESIAN_POINT ( 'NONE',  ( 3.272451888078301785, -24.83884780301426787, 145.0000119999999697 ) ) ;
#13074 = CIRCLE ( 'NONE', #12697, 4.000000000000000000 ) ;
#13075 = CIRCLE ( 'NONE', #11131, 25.00000000000000000 ) ;
#13076 = AXIS2_PLACEMENT_3D ( 'NONE', #7915, #13747, #11577 ) ;
#13077 = EDGE_LOOP ( 'NONE', ( #8030, #2406 ) ) ;
#13078 = CARTESIAN_POINT ( 'NONE',  ( 0.000000000000000000, -131.7994082814339833, 3.000000000000000000 ) ) ;
#13079 = VECTOR ( 'NONE', #3162, 1000.000000000000000 ) ;
#13080 = CARTESIAN_POINT ( 'NONE',  ( 312.2000000000013529, -132.2000000000000455, 146.4928932188134638 ) ) ;
#13081 = ORIENTED_EDGE ( 'NONE', *, *, #7252, .F. ) ;
#13082 = CARTESIAN_POINT ( 'NONE',  ( -0.3483149870578547969, 8.861353789385022495, -7.493854785173811983 ) ) ;
#13083 = EDGE_LOOP ( 'NONE', ( #2367, #21884, #11640, #23632 ) ) ;
#13084 = CARTESIAN_POINT ( 'NONE',  ( -31.74999999999995737, 0.000000000000000000, 0.000000000000000000 ) ) ;
#13085 = FACE_OUTER_BOUND ( 'NONE', #18646, .T. ) ;
#13086 = ORIENTED_EDGE ( 'NONE', *, *, #13936, .F. ) ;
#13087 = CARTESIAN_POINT ( 'NONE',  ( -4.606548227981510202, -6.456511556909259930, -7.591235721156638583 ) ) ;
#13088 = CARTESIAN_POINT ( 'NONE',  ( 65.00000000000002842, -56.79999999999928662, 155.0000000000002558 ) ) ;
#13089 = EDGE_CURVE ( 'NONE', #6451, #18839, #22871, .T. ) ;
#13090 = CONICAL_SURFACE ( 'NONE', #17299, 7.500000000000001776, 0.8594454914424796144 ) ;
#13091 = VECTOR ( 'NONE', #17703, 1000.000000000000114 ) ;
#13092 = SURFACE_STYLE_USAGE ( .BOTH. , #11276 ) ;
#13093 = EDGE_CURVE ( 'NONE', #5216, #18725, #8388, .T. ) ;
#13094 = VECTOR ( 'NONE', #1719, 1000.000000000000000 ) ;
#13095 = CARTESIAN_POINT ( 'NONE',  ( 281.6810649015077388, 272.7324007871374079, 145.3120962995435832 ) ) ;
#13096 = CARTESIAN_POINT ( 'NONE',  ( 124.4701338314433201, -1092.369831568443260, -32.49999999999351985 ) ) ;
#13097 = AXIS2_PLACEMENT_3D ( 'NONE', #2370, #2239, #8185 ) ;
#13098 = EDGE_CURVE ( 'NONE', #14948, #17788, #2490, .T. ) ;
#13099 = CARTESIAN_POINT ( 'NONE',  ( -7.500000000000001776, 0.000000000000000000, 0.000000000000000000 ) ) ;
#13100 = ORIENTED_EDGE ( 'NONE', *, *, #9906, .F. ) ;
#13101 = CARTESIAN_POINT ( 'NONE',  ( 119.6158142514527469, -1087.367367941136308, 27.94500000000641649 ) ) ;
#13102 = CARTESIAN_POINT ( 'NONE',  ( -282.2000000000012960, -74.99999999999899103, 90.00000000000000000 ) ) ;
#13104 = ORIENTED_EDGE ( 'NONE', *, *, #4552, .T. ) ;
#13103 = EDGE_LOOP ( 'NONE', ( #19030, #22049, #2030, #2379 ) ) ;
#13105 = DIRECTION ( 'NONE',  ( 1.000000000000000000, 0.000000000000000000, 0.000000000000000000 ) ) ;
#13106 = CARTESIAN_POINT ( 'NONE',  ( -136.5854636148305019, -1073.276359373527612, -31.88829724122658860 ) ) ;
#13107 = CARTESIAN_POINT ( 'NONE',  ( 32.35000000000001563, 90.00000000000000000, 0.000000000000000000 ) ) ;
#13108 = ORIENTED_EDGE ( 'NONE', *, *, #19832, .T. ) ;
#13109 = CIRCLE ( 'NONE', #20778, 160.0000000000000000 ) ;
#13110 = CARTESIAN_POINT ( 'NONE',  ( -44.99999999999995026, -59.79999999999968452, 105.0000000000002274 ) ) ;
#13112 = AXIS2_PLACEMENT_3D ( 'NONE', #14824, #13166, #14943 ) ;
#13111 = STYLED_ITEM ( 'NONE', ( #13334 ), #8186 ) ;
#13113 = VERTEX_POINT ( 'NONE', #4409 ) ;
#13114 = VECTOR ( 'NONE', #10747, 1000.000000000000000 ) ;
#13115 = VECTOR ( 'NONE', #18158, 1000.000000000000000 ) ;
#13116 = CIRCLE ( 'NONE', #3020, 5.199999999999982414 ) ;
#13117 = DIRECTION ( 'NONE',  ( -0.000000000000000000, -0.000000000000000000, -1.000000000000000000 ) ) ;
#13118 = VECTOR ( 'NONE', #19819, 1000.000000000000000 ) ;
#13119 = VERTEX_POINT ( 'NONE', #11940 ) ;
#13120 = CARTESIAN_POINT ( 'NONE',  ( -282.2000000000006708, 90.00000000000100897, 34.99999999999999289 ) ) ;
#13121 = CIRCLE ( 'NONE', #22703, 25.00000000000000000 ) ;
#13122 = ORIENTED_EDGE ( 'NONE', *, *, #8970, .F. ) ;
#13123 = APPLICATION_CONTEXT ( 'automotive_design' ) ;
#13124 = CARTESIAN_POINT ( 'NONE',  ( 125.8126197883822641, -1090.532805371500217, 31.11671059283543528 ) ) ;
#13125 = ORIENTED_EDGE ( 'NONE', *, *, #20664, .T. ) ;
#13126 = CARTESIAN_POINT ( 'NONE',  ( -129.1735827702802055, 85.66907061909537902, 31.11671059283535712 ) ) ;
#13127 = DIRECTION ( 'NONE',  ( -0.000000000000000000, -0.000000000000000000, -1.000000000000000000 ) ) ;
#13128 = EDGE_CURVE ( 'NONE', #11691, #15468, #11009, .T. ) ;
#13129 = CARTESIAN_POINT ( 'NONE',  ( 4.197310751797292738, 0.8178363989516252985, -3.502498386812444409 ) ) ;
#13130 = CIRCLE ( 'NONE', #2668, 2.499999999999998668 ) ;
#13131 = AXIS2_PLACEMENT_3D ( 'NONE', #18605, #11050, #5701 ) ;
#13132 = CARTESIAN_POINT ( 'NONE',  ( 155.0000000000000284, -500.0000000000000000, -29.99999999999997158 ) ) ;
#13133 = VECTOR ( 'NONE', #15739, 1000.000000000000000 ) ;
#13134 = CARTESIAN_POINT ( 'NONE',  ( -280.5743436287469308, 269.9433523009093392, 145.2481149223240777 ) ) ;
#13135 = AXIS2_PLACEMENT_3D ( 'NONE', #7434, #20703, #7916 ) ;
#13136 = CARTESIAN_POINT ( 'NONE',  ( 2.500000000000000000, 2.357898499370433054, -1.951563910473907981E-15 ) ) ;
#13137 = AXIS2_PLACEMENT_3D ( 'NONE', #19133, #13394, #2728 ) ;
#13138 = CIRCLE ( 'NONE', #2675, 7.500000000000001776 ) ;
#13139 = CONICAL_SURFACE ( 'NONE', #4592, 2.055000000000001492, 0.7853981633974633780 ) ;
#13140 = VECTOR ( 'NONE', #20643, 1000.000000000000000 ) ;
#13141 = EDGE_LOOP ( 'NONE', ( #18276, #7970, #17475, #12084 ) ) ;
#13142 = CARTESIAN_POINT ( 'NONE',  ( -7.922281120364393914, -4.573931137438277617, -8.047472243342932430 ) ) ;
#13143 = CARTESIAN_POINT ( 'NONE',  ( 132.1831532210149476, 80.94878845338332951, -27.81095155082709525 ) ) ;
#13144 = PLANE ( 'NONE',  #8865 ) ;
#13145 = CARTESIAN_POINT ( 'NONE',  ( 100.0000000000000000, 269.9999999999999432, 125.0000000000000284 ) ) ;
#13147 = VECTOR ( 'NONE', #21128, 1000.000000000000000 ) ;
#13146 = AXIS2_PLACEMENT_3D ( 'NONE', #8367, #10804, #6677 ) ;
#13148 = DIRECTION ( 'NONE',  ( 0.000000000000000000, 0.8660254037844380415, -0.5000000000000011102 ) ) ;
#13149 = CARTESIAN_POINT ( 'NONE',  ( -280.6822561791012731, 272.9663407402829876, -145.1247002395579671 ) ) ;
#13150 = PRESENTATION_LAYER_ASSIGNMENT (  '', '', ( #23524 ) ) ;
#13151 = AXIS2_PLACEMENT_3D ( 'NONE', #1468, #10564, #14420 ) ;
#13152 = VERTEX_POINT ( 'NONE', #12179 ) ;
#13153 = AXIS2_PLACEMENT_3D ( 'NONE', #4090, #720, #15354 ) ;
#13154 = VECTOR ( 'NONE', #16161, 1000.000000000000114 ) ;
#13155 = CARTESIAN_POINT ( 'NONE',  ( 1.636246173744675403, -975.0000000000000000, 145.0000119999999697 ) ) ;
#13156 = ORIENTED_EDGE ( 'NONE', *, *, #23556, .T. ) ;
#13157 = CARTESIAN_POINT ( 'NONE',  ( 110.0000000000000000, -74.99999999999998579, 3.000000000000000000 ) ) ;
#13158 = LINE ( 'NONE', #7664, #21792 ) ;
#13159 = DIRECTION ( 'NONE',  ( -0.9423651898111409242, -0.3345860861306287903, 6.982962677686267499E-15 ) ) ;
#13160 = ORIENTED_EDGE ( 'NONE', *, *, #13496, .F. ) ;
#13161 = DIRECTION ( 'NONE',  ( -0.000000000000000000, -0.000000000000000000, 1.000000000000000000 ) ) ;
#13162 = CARTESIAN_POINT ( 'NONE',  ( 123.1514321905979443, -1094.120844545942873, -31.25955389945132268 ) ) ;
#13163 = ADVANCED_FACE ( 'NONE', ( #11701 ), #20841, .F. ) ;
#13164 = DIRECTION ( 'NONE',  ( -1.000000000000000000, -0.000000000000000000, -0.000000000000000000 ) ) ;
#13165 = DIRECTION ( 'NONE',  ( -0.000000000000000000, -0.000000000000000000, 1.000000000000000000 ) ) ;
#13166 = DIRECTION ( 'NONE',  ( 0.000000000000000000, -1.177509268541832635E-16, 1.000000000000000000 ) ) ;
#13167 = CARTESIAN_POINT ( 'NONE',  ( -1.118033988749894458, 0.000000000000000000, -21.50000000000000000 ) ) ;
#13168 = EDGE_CURVE ( 'NONE', #6672, #12336, #670, .T. ) ;
#13169 = CARTESIAN_POINT ( 'NONE',  ( 2.500000000000000000, -2.629050547790028551E-15, -2.041999999999999815 ) ) ;
#13170 = EDGE_LOOP ( 'NONE', ( #7353, #5253 ) ) ;
#13171 = AXIS2_PLACEMENT_3D ( 'NONE', #14038, #6757, #10765 ) ;
#13172 = DIRECTION ( 'NONE',  ( 0.000000000000000000, 3.483493295888648978E-15, 1.000000000000000000 ) ) ;
#13173 = CYLINDRICAL_SURFACE ( 'NONE', #11622, 5.249999999999942268 ) ;
#13174 = ADVANCED_FACE ( 'NONE', ( #1146 ), #8525, .F. ) ;
#13175 = VECTOR ( 'NONE', #20238, 1000.000000000000000 ) ;
#13176 = ORIENTED_EDGE ( 'NONE', *, *, #116, .T. ) ;
#13177 = AXIS2_PLACEMENT_3D ( 'NONE', #9526, #7580, #20371 ) ;
#13178 = AXIS2_PLACEMENT_3D ( 'NONE', #11232, #2115, #677 ) ;
#13179 = DIRECTION ( 'NONE',  ( -1.000000000000000000, -3.491481338843133355E-15, 0.000000000000000000 ) ) ;
#13180 = CARTESIAN_POINT ( 'NONE',  ( 100.0000000000000000, -1400.000000000000000, -125.0000000000001705 ) ) ;
#13181 = DIRECTION ( 'NONE',  ( 0.000000000000000000, -1.000000000000000000, -5.286776307738891306E-15 ) ) ;
#13182 = ADVANCED_FACE ( 'NONE', ( #6341 ), #9864, .T. ) ;
#13183 = ORIENTED_EDGE ( 'NONE', *, *, #23803, .F. ) ;
#13184 = DIRECTION ( 'NONE',  ( 0.000000000000000000, 1.000000000000000000, -3.502807018799300809E-15 ) ) ;
#13185 = CARTESIAN_POINT ( 'NONE',  ( 0.6508621380849231031, 8.763657152406445050, -7.907633014911220393 ) ) ;
#13186 = CARTESIAN_POINT ( 'NONE',  ( 5.000000000000000000, 4.685197434473814759, -5.637851296924623057E-15 ) ) ;
#13187 = ORIENTED_EDGE ( 'NONE', *, *, #17688, .T. ) ;
#13188 = CARTESIAN_POINT ( 'NONE',  ( 279.9999999999999432, 272.9999999999999432, 145.0000000000000284 ) ) ;
#13189 = DIRECTION ( 'NONE',  ( 0.000000000000000000, 0.000000000000000000, -1.000000000000000000 ) ) ;
#13190 = DIRECTION ( 'NONE',  ( 0.000000000000000000, 0.000000000000000000, 1.000000000000000000 ) ) ;
#13191 = DIRECTION ( 'NONE',  ( 0.000000000000000000, 0.000000000000000000, 1.000000000000000000 ) ) ;
#13192 = EDGE_LOOP ( 'NONE', ( #6222, #5909, #23392, #12079 ) ) ;
#13193 = CARTESIAN_POINT ( 'NONE',  ( 279.9999999999999432, 273.0299999999999159, -144.9999999999999716 ) ) ;
#13194 = APPLICATION_PROTOCOL_DEFINITION ( 'draft international standard', 'automotive_design', 1998, #7365 ) ;
#13195 = DIRECTION ( 'NONE',  ( 1.000000000000000000, 0.000000000000000000, 0.000000000000000000 ) ) ;
#13196 = CARTESIAN_POINT ( 'NONE',  ( -6.625705691649848461, 5.306270977113102916, -7.795653906409009792 ) ) ;
#13197 = CARTESIAN_POINT ( 'NONE',  ( -312.2000000000014666, -132.2000000000000455, 146.4928932188134638 ) ) ;
#13198 = VERTEX_POINT ( 'NONE', #2724 ) ;
#13199 = VERTEX_POINT ( 'NONE', #8042 ) ;
#13200 = FACE_OUTER_BOUND ( 'NONE', #9359, .T. ) ;
#13201 = CARTESIAN_POINT ( 'NONE',  ( 146.0000000000002274, -210.0000000000003411, -29.99999999999356604 ) ) ;
#13202 = EDGE_CURVE ( 'NONE', #2178, #16805, #15611, .T. ) ;
#13203 = EDGE_CURVE ( 'NONE', #8986, #12593, #19131, .T. ) ;
#13204 = EDGE_CURVE ( 'NONE', #22628, #14701, #17456, .T. ) ;
#13205 = DIRECTION ( 'NONE',  ( 0.000000000000000000, 1.000000000000000000, 0.000000000000000000 ) ) ;
#13206 = ADVANCED_FACE ( 'NONE', ( #8281 ), #18048, .F. ) ;
#13207 = DIRECTION ( 'NONE',  ( 0.000000000000000000, 0.000000000000000000, 1.000000000000000000 ) ) ;
#13208 = EDGE_CURVE ( 'NONE', #9513, #12624, #10706, .T. ) ;
#13209 = VERTEX_POINT ( 'NONE', #10476 ) ;
#13211 = ADVANCED_FACE ( 'NONE', ( #3071 ), #20209, .T. ) ;
#13210 = FACE_OUTER_BOUND ( 'NONE', #10142, .T. ) ;
#13212 = ORIENTED_EDGE ( 'NONE', *, *, #15885, .F. ) ;
#13213 = DIRECTION ( 'NONE',  ( 0.000000000000000000, 0.000000000000000000, -1.000000000000000000 ) ) ;
#13214 = FACE_OUTER_BOUND ( 'NONE', #15092, .T. ) ;
#13215 = ORIENTED_EDGE ( 'NONE', *, *, #2996, .F. ) ;
#13216 = CARTESIAN_POINT ( 'NONE',  ( -129.0269476471444534, 85.88978664864571044, -28.46728581292316207 ) ) ;
#13217 = DIRECTION ( 'NONE',  ( 1.000000000000000000, 0.000000000000000000, 0.000000000000000000 ) ) ;
#13218 = CARTESIAN_POINT ( 'NONE',  ( 23.72315261474501469, -1008.055391459054249, 145.0000119999999697 ) ) ;
#13219 = CARTESIAN_POINT ( 'NONE',  ( 285.1999999999998181, 268.1431883566700662, 146.4301685943532334 ) ) ;
#13220 = CARTESIAN_POINT ( 'NONE',  ( 24.99999999999998224, -1000.000000000000000, 145.0000059999999280 ) ) ;
#13221 = CARTESIAN_POINT ( 'NONE',  ( 0.000000000000000000, -2.357898499370432610, 3.252606517456513302E-15 ) ) ;
#13222 = FACE_OUTER_BOUND ( 'NONE', #8685, .T. ) ;
#13223 = EDGE_LOOP ( 'NONE', ( #4077, #14105, #15838, #12175 ) ) ;
#13224 = DIRECTION ( 'NONE',  ( 0.000000000000000000, 0.000000000000000000, -1.000000000000000000 ) ) ;
#13226 = EDGE_LOOP ( 'NONE', ( #6287, #17828, #17651, #17608 ) ) ;
#13225 = VERTEX_POINT ( 'NONE', #18167 ) ;
#13227 = DIRECTION ( 'NONE',  ( 5.135813185032629306E-32, -1.850371707708594366E-15, -1.000000000000000000 ) ) ;
#13228 = CARTESIAN_POINT ( 'NONE',  ( 279.9999999999999432, 273.0000000000000000, -144.9999999999999716 ) ) ;
#13229 = VERTEX_POINT ( 'NONE', #18270 ) ;
#13230 = CARTESIAN_POINT ( 'NONE',  ( -135.1739945062388415, -1075.849084086416042, 32.18904844917291541 ) ) ;
#13231 = EDGE_CURVE ( 'NONE', #18285, #19306, #930, .T. ) ;
#13232 = ADVANCED_FACE ( 'NONE', ( #19962 ), #8889, .F. ) ;
#13233 = ORIENTED_EDGE ( 'NONE', *, *, #20849, .F. ) ;
#13234 = EDGE_CURVE ( 'NONE', #10308, #22960, #6816, .T. ) ;
#13235 = CARTESIAN_POINT ( 'NONE',  ( 284.6728700860325034, 270.1062614524586252, -146.0570750465943206 ) ) ;
#13236 = VERTEX_POINT ( 'NONE', #21780 ) ;
#13237 = DIRECTION ( 'NONE',  ( 1.000000000000000000, -0.000000000000000000, 6.982962677686266711E-15 ) ) ;
#13238 = PLANE ( 'NONE',  #16557 ) ;
#13239 = ITEM_DEFINED_TRANSFORMATION ( 'NONE', 'NONE', #3482,  #11210 ) ;
#13240 = ORIENTED_EDGE ( 'NONE', *, *, #19348, .F. ) ;
#13241 = B_SPLINE_CURVE_WITH_KNOTS ( 'NONE', 3,
 ( #13311, #20622, #11630, #17029, #482, #7591 ),
 .UNSPECIFIED., .F., .F.,
 ( 4, 2, 4 ),
 ( 0.004444412883774350592, 0.006655097293744440673, 0.008865781703714530754 ),
 .UNSPECIFIED. ) ;
#13242 = CARTESIAN_POINT ( 'NONE',  ( 119.9257125005558606, -1087.686723660049893, 30.00000000000641975 ) ) ;
#13243 = ORIENTED_EDGE ( 'NONE', *, *, #13089, .F. ) ;
#13244 = CARTESIAN_POINT ( 'NONE',  ( -129.1300454301538707, 85.73470730629014724, 31.26048023074367421 ) ) ;
#13245 = CARTESIAN_POINT ( 'NONE',  ( -1.393927851585477606, 4.043713361053528743, -3.526374918436835149 ) ) ;
#13246 = CARTESIAN_POINT ( 'NONE',  ( 4.000000000000000000, 2.309401076758497151, -5.000000000000000000 ) ) ;
#13247 = B_SPLINE_CURVE_WITH_KNOTS ( 'NONE', 3,
 ( #16624, #3555, #10727, #76, #9132 ),
 .UNSPECIFIED., .F., .F.,
 ( 4, 1, 4 ),
 ( 5.640274452250024914E-20, 0.002309401076758505356, 0.004618802153517010713 ),
 .UNSPECIFIED. ) ;
#13248 = DIRECTION ( 'NONE',  ( 1.000000000000000000, -0.000000000000000000, -0.000000000000000000 ) ) ;
#13249 = VERTEX_POINT ( 'NONE', #23354 ) ;
#13250 = CARTESIAN_POINT ( 'NONE',  ( -280.4976310729378497, 269.7223300543793698, -146.1079617568159392 ) ) ;
#13251 = DIRECTION ( 'NONE',  ( 1.000000000000000000, 0.000000000000000000, 0.000000000000000000 ) ) ;
#13252 = VERTEX_POINT ( 'NONE', #14552 ) ;
#13253 = CARTESIAN_POINT ( 'NONE',  ( 163.0000000000002558, -500.0000000000003411, -29.99999999999344880 ) ) ;
#13254 = FACE_OUTER_BOUND ( 'NONE', #8183, .T. ) ;
#13255 = DIRECTION ( 'NONE',  ( 1.000000000000000000, -0.000000000000000000, 6.982962677686266711E-15 ) ) ;
#13256 = CARTESIAN_POINT ( 'NONE',  ( 281.3689414351989626, 272.8938770989752811, 145.2488155364688964 ) ) ;
#13257 = DIRECTION ( 'NONE',  ( -0.000000000000000000, -0.000000000000000000, 1.000000000000000000 ) ) ;
#13258 = AXIS2_PLACEMENT_3D ( 'NONE', #22073, #9059, #20257 ) ;
#13259 = CARTESIAN_POINT ( 'NONE',  ( 2.500000000000000000, 2.357898499370431722, -2.818925648462311528E-15 ) ) ;
#13260 = CARTESIAN_POINT ( 'NONE',  ( 124.0809974055277678, -1092.892044598689608, 27.57867027829822959 ) ) ;
#13261 = ITEM_DEFINED_TRANSFORMATION ( 'NONE', 'NONE', #10829,  #11210 ) ;
#13262 = ORIENTED_EDGE ( 'NONE', *, *, #3250, .T. ) ;
#13263 = CARTESIAN_POINT ( 'NONE',  ( 0.000000000000000000, 0.000000000000000000, -100.0000000000000000 ) ) ;
#13264 = ORIENTED_EDGE ( 'NONE', *, *, #9319, .T. ) ;
#13265 = CARTESIAN_POINT ( 'NONE',  ( 0.2500000000000002220, 0.000000000000000000, 4.250000000000000000 ) ) ;
#13266 = DIRECTION ( 'NONE',  ( 1.000000000000000000, 3.469446951953626515E-16, 3.469446951953613203E-16 ) ) ;
#13267 = PLANE ( 'NONE',  #2487 ) ;
#13268 = ORIENTED_EDGE ( 'NONE', *, *, #5917, .T. ) ;
#13269 = FACE_OUTER_BOUND ( 'NONE', #8056, .T. ) ;
#13270 = FACE_OUTER_BOUND ( 'NONE', #12693, .T. ) ;
#13271 = CARTESIAN_POINT ( 'NONE',  ( -24.99999999999998224, -1000.000000000000000, -138.9999999999999716 ) ) ;
#13272 = DIRECTION ( 'NONE',  ( 0.000000000000000000, 0.000000000000000000, 1.000000000000000000 ) ) ;
#13273 = CARTESIAN_POINT ( 'NONE',  ( -1.500000000000000000, 0.000000000000000000, 0.000000000000000000 ) ) ;
#13274 = DIRECTION ( 'NONE',  ( -1.000000000000000000, -0.000000000000000000, -0.000000000000000000 ) ) ;
#13275 = CARTESIAN_POINT ( 'NONE',  ( -7.922811899608408481, -4.628803996615321381, -8.057669882367649805 ) ) ;
#13276 = VECTOR ( 'NONE', #6110, 1000.000000000000000 ) ;
#13277 = ORIENTED_EDGE ( 'NONE', *, *, #4460, .T. ) ;
#13278 = LINE ( 'NONE', #7559, #5698 ) ;
#13279 = CARTESIAN_POINT ( 'NONE',  ( 0.000000000000000000, 1.865214261513747767E-15, 138.9999999999999716 ) ) ;
#13280 = ORIENTED_EDGE ( 'NONE', *, *, #20532, .F. ) ;
#13281 = EDGE_CURVE ( 'NONE', #18427, #13434, #5187, .T. ) ;
#13282 = VERTEX_POINT ( 'NONE', #12428 ) ;
#13283 = CARTESIAN_POINT ( 'NONE',  ( -281.4928932188135491, -127.0000000000000568, 147.2000000000013813 ) ) ;
#13284 = CARTESIAN_POINT ( 'NONE',  ( 2.500000000000000000, 0.000000000000000000, 0.000000000000000000 ) ) ;
#13285 = CARTESIAN_POINT ( 'NONE',  ( 279.9999999999999432, 269.9999999999999432, -144.9999999999999716 ) ) ;
#13286 = AXIS2_PLACEMENT_3D ( 'NONE', #17149, #375, #7478 ) ;
#13287 = EDGE_CURVE ( 'NONE', #21638, #20769, #11377, .T. ) ;
#13288 = VECTOR ( 'NONE', #23593, 1000.000000000000000 ) ;
#13289 = ORIENTED_EDGE ( 'NONE', *, *, #18314, .F. ) ;
#13290 = DIRECTION ( 'NONE',  ( 0.000000000000000000, 0.000000000000000000, -1.000000000000000000 ) ) ;
#13291 = CARTESIAN_POINT ( 'NONE',  ( 5.274401269815139237, 6.074457022762083547, -7.633824513837111247 ) ) ;
#13292 = ADVANCED_FACE ( 'NONE', ( #10590 ), #5571, .T. ) ;
#13293 = CARTESIAN_POINT ( 'NONE',  ( -6.145467199749147902, -7.996668423981801332, 200.0000120000000265 ) ) ;
#13294 = VERTEX_POINT ( 'NONE', #21668 ) ;
#13295 = CARTESIAN_POINT ( 'NONE',  ( 280.9953931959806255, 270.4054396500290522, 149.5132312761074331 ) ) ;
#13296 = DIRECTION ( 'NONE',  ( -1.000000000000000000, -0.000000000000000000, -0.000000000000000000 ) ) ;
#13297 = EDGE_CURVE ( 'NONE', #10308, #20252, #12787, .T. ) ;
#13298 = ORIENTED_EDGE ( 'NONE', *, *, #22597, .T. ) ;
#13299 = CARTESIAN_POINT ( 'NONE',  ( 5.200000000000002842, 0.000000000000000000, -2.700000000000000622 ) ) ;
#13300 = SHAPE_DEFINITION_REPRESENTATION ( #12136, #19462 ) ;
#13301 = DIRECTION ( 'NONE',  ( -0.000000000000000000, 1.000000000000000000, -3.469446951953613794E-15 ) ) ;
#13302 = CARTESIAN_POINT ( 'NONE',  ( -7.970070017554212960, 4.546953124339755625, -8.057670357645356773 ) ) ;
#13303 = CARTESIAN_POINT ( 'NONE',  ( -105.0000000000000000, -29.99999999999998579, 3.000000000000000000 ) ) ;
#13304 = CIRCLE ( 'NONE', #19022, 5.249999999999962697 ) ;
#13305 = ORIENTED_EDGE ( 'NONE', *, *, #2648, .F. ) ;
#13306 = AXIS2_PLACEMENT_3D ( 'NONE', #15303, #18539, #16739 ) ;
#13307 = VERTEX_POINT ( 'NONE', #5126 ) ;
#13308 = LINE ( 'NONE', #18933, #3734 ) ;
#13309 = DIRECTION ( 'NONE',  ( 0.000000000000000000, -0.000000000000000000, 1.000000000000000000 ) ) ;
#13310 = ORIENTED_EDGE ( 'NONE', *, *, #1310, .F. ) ;
#13311 = CARTESIAN_POINT ( 'NONE',  ( -3.750000000000007105, -6.495190528383289141, 0.000000000000000000 ) ) ;
#13312 = DIRECTION ( 'NONE',  ( 0.000000000000000000, -0.5000000000000011102, -0.8660254037844379305 ) ) ;
#13313 = ORIENTED_EDGE ( 'NONE', *, *, #7841, .F. ) ;
#13314 = DIRECTION ( 'NONE',  ( -1.000000000000000000, 0.000000000000000000, 0.000000000000000000 ) ) ;
#13315 = PRESENTATION_LAYER_ASSIGNMENT (  '', '', ( #6329 ) ) ;
#13316 = ORIENTED_EDGE ( 'NONE', *, *, #872, .T. ) ;
#13317 = CARTESIAN_POINT ( 'NONE',  ( 2.500000000000000000, 0.000000000000000000, 0.000000000000000000 ) ) ;
#13318 = EDGE_CURVE ( 'NONE', #9978, #16229, #23596, .T. ) ;
#13319 = CYLINDRICAL_SURFACE ( 'NONE', #23664, 2.500000000000002220 ) ;
#13320 = VERTEX_POINT ( 'NONE', #3299 ) ;
#13321 = VERTEX_POINT ( 'NONE', #17813 ) ;
#13322 = CARTESIAN_POINT ( 'NONE',  ( 126.7787238282401461, 77.44864885511553609, -29.99999999999356248 ) ) ;
#13323 = ADVANCED_FACE ( 'NONE', ( #20091 ), #17147, .F. ) ;
#13324 = CARTESIAN_POINT ( 'NONE',  ( -280.2489140339770302, 272.8335297745771300, -146.3488036478619847 ) ) ;
#13325 = CYLINDRICAL_SURFACE ( 'NONE', #15217, 2.649999999999985700 ) ;
#13326 = CARTESIAN_POINT ( 'NONE',  ( 283.1755088701071941, 271.9320353020569883, 145.6228333615950419 ) ) ;
#13327 = CARTESIAN_POINT ( 'NONE',  ( 24.20041621714722879, -993.5179357872714263, 145.0000119999999413 ) ) ;
#13328 = DIRECTION ( 'NONE',  ( -0.000000000000000000, 1.000000000000000000, -0.000000000000000000 ) ) ;
#13329 = EDGE_CURVE ( 'NONE', #3759, #18160, #12651, .T. ) ;
#13330 = DIRECTION ( 'NONE',  ( 0.000000000000000000, 0.000000000000000000, 1.000000000000000000 ) ) ;
#13331 = VERTEX_POINT ( 'NONE', #23231 ) ;
#13332 = LINE ( 'NONE', #13101, #16113 ) ;
#13333 = FACE_OUTER_BOUND ( 'NONE', #2421, .T. ) ;
#13334 = PRESENTATION_STYLE_ASSIGNMENT (( #5927 ) ) ;
#13335 = EDGE_CURVE ( 'NONE', #4538, #23797, #6701, .T. ) ;
#13337 = VERTEX_POINT ( 'NONE', #1261 ) ;
#13336 = ORIENTED_EDGE ( 'NONE', *, *, #10514, .F. ) ;
#13338 = AXIS2_PLACEMENT_3D ( 'NONE', #16674, #2036, #20753 ) ;
#13339 = DIRECTION ( 'NONE',  ( -0.000000000000000000, -0.000000000000000000, 1.000000000000000000 ) ) ;
#13340 = CARTESIAN_POINT ( 'NONE',  ( 280.1244266708878285, 270.0000000000000000, -145.2880230824753198 ) ) ;
#13341 = VECTOR ( 'NONE', #9192, 1000.000000000000000 ) ;
#13342 = ORIENTED_EDGE ( 'NONE', *, *, #1307, .F. ) ;
#13343 = AXIS2_PLACEMENT_3D ( 'NONE', #1164, #2606, #15672 ) ;
#13344 = FACE_OUTER_BOUND ( 'NONE', #825, .T. ) ;
#13345 = ORIENTED_EDGE ( 'NONE', *, *, #22168, .F. ) ;
#13346 = CARTESIAN_POINT ( 'NONE',  ( 145.9999999999998010, -801.0618695410399823, 30.00000000000641620 ) ) ;
#13347 = ORIENTED_EDGE ( 'NONE', *, *, #23734, .F. ) ;
#13348 = EDGE_CURVE ( 'NONE', #10540, #6672, #6736, .T. ) ;
#13349 = AXIS2_PLACEMENT_3D ( 'NONE', #1091, #22830, #17296 ) ;
#13350 = CARTESIAN_POINT ( 'NONE',  ( 100.0000000000000000, 250.0000000000000000, -124.9999999999999716 ) ) ;
#13351 = EDGE_LOOP ( 'NONE', ( #9038, #9219 ) ) ;
#13352 = CIRCLE ( 'NONE', #6371, 2.649999999999985700 ) ;
#13353 = DIRECTION ( 'NONE',  ( -3.736327486719275871E-16, 1.000000000000000000, 0.000000000000000000 ) ) ;
#13354 = EDGE_LOOP ( 'NONE', ( #126, #739, #15782 ) ) ;
#13355 = CARTESIAN_POINT ( 'NONE',  ( -19.87452195017631595, -984.7454242570835277, -145.0000000000001137 ) ) ;
#13356 = CARTESIAN_POINT ( 'NONE',  ( -2.805705207896067144, 3.226868319750155312, -3.503898532754364581 ) ) ;
#13357 = CIRCLE ( 'NONE', #207, 5.249999999999956479 ) ;
#13358 = DIRECTION ( 'NONE',  ( 0.000000000000000000, 0.000000000000000000, -1.000000000000000000 ) ) ;
#13359 = DIRECTION ( 'NONE',  ( 0.000000000000000000, 0.000000000000000000, -1.000000000000000000 ) ) ;
#13360 = ADVANCED_FACE ( 'NONE', ( #22123, #4004 ), #16604, .T. ) ;
#13361 = VERTEX_POINT ( 'NONE', #11308 ) ;
#13362 = CARTESIAN_POINT ( 'NONE',  ( -280.6220388411722411, 271.9582675804705332, -148.1956429438695579 ) ) ;
#13363 = ADVANCED_FACE ( 'NONE', ( #166 ), #19043, .F. ) ;
#13364 =( LENGTH_UNIT ( ) NAMED_UNIT ( * ) SI_UNIT ( .MILLI., .METRE. ) );
#13365 = ORIENTED_EDGE ( 'NONE', *, *, #18670, .F. ) ;
#13366 = DIRECTION ( 'NONE',  ( -1.000000000000000000, 0.000000000000000000, -6.982962677686266711E-15 ) ) ;
#13367 = LINE ( 'NONE', #5719, #22674 ) ;
#13368 = VECTOR ( 'NONE', #12320, 1000.000000000000114 ) ;
#13369 = DIRECTION ( 'NONE',  ( 0.000000000000000000, 0.000000000000000000, 1.000000000000000000 ) ) ;
#13370 = CARTESIAN_POINT ( 'NONE',  ( 282.6339272673396863, 272.3699028110927429, 145.4976310729378497 ) ) ;
#13371 = AXIS2_PLACEMENT_3D ( 'NONE', #11747, #22444, #4082 ) ;
#13372 = FACE_OUTER_BOUND ( 'NONE', #7809, .T. ) ;
#13373 = EDGE_LOOP ( 'NONE', ( #17256, #10802 ) ) ;
#13374 = VECTOR ( 'NONE', #18162, 1000.000000000000000 ) ;
#13375 = CARTESIAN_POINT ( 'NONE',  ( 235.0000000000000284, -560.0000000000000000, -60.00000000000000711 ) ) ;
#13376 = CARTESIAN_POINT ( 'NONE',  ( 26.98333333333332007, -89.99999999999998579, 3.000000000000001332 ) ) ;
#13377 = CARTESIAN_POINT ( 'NONE',  ( 122.9870427404262045, -1094.335589877584425, 29.33965772977896691 ) ) ;
#13378 = ORIENTED_EDGE ( 'NONE', *, *, #10465, .T. ) ;
#13379 = DIRECTION ( 'NONE',  ( 1.000000000000000000, -0.000000000000000000, 6.982962677686266711E-15 ) ) ;
#13380 = VERTEX_POINT ( 'NONE', #5596 ) ;
#13382 = ADVANCED_FACE ( 'NONE', ( #11422 ), #5840, .F. ) ;
#13381 = FACE_BOUND ( 'NONE', #3876, .T. ) ;
#13383 = DIRECTION ( 'NONE',  ( 0.000000000000000000, -1.000000000000000000, -3.495664435217746987E-15 ) ) ;
#13384 = VERTEX_POINT ( 'NONE', #7772 ) ;
#13385 = AXIS2_PLACEMENT_3D ( 'NONE', #11797, #13257, #22744 ) ;
#13386 = DIRECTION ( 'NONE',  ( 0.000000000000000000, 0.000000000000000000, -1.000000000000000000 ) ) ;
#13387 = ORIENTED_EDGE ( 'NONE', *, *, #21677, .T. ) ;
#13388 = FACE_OUTER_BOUND ( 'NONE', #19941, .T. ) ;
#13389 = CARTESIAN_POINT ( 'NONE',  ( 235.0000000000000284, -500.0000000000000000, 60.00000000000002132 ) ) ;
#13390 = DIRECTION ( 'NONE',  ( 1.000000000000000000, 0.000000000000000000, 0.000000000000000000 ) ) ;
#13391 = DIRECTION ( 'NONE',  ( 0.000000000000000000, -3.495664435217746987E-15, 1.000000000000000000 ) ) ;
#13392 = EDGE_CURVE ( 'NONE', #12336, #2069, #10211, .T. ) ;
#13393 = DIRECTION ( 'NONE',  ( 1.000000000000000000, -0.000000000000000000, -0.000000000000000000 ) ) ;
#13394 = DIRECTION ( 'NONE',  ( 0.000000000000000000, 0.000000000000000000, 1.000000000000000000 ) ) ;
#13395 = LINE ( 'NONE', #20341, #1284 ) ;
#13396 = EDGE_CURVE ( 'NONE', #18184, #9858, #1317, .T. ) ;
#13397 = VERTEX_POINT ( 'NONE', #11537 ) ;
#13398 = DIRECTION ( 'NONE',  ( -1.000000000000000000, 7.709882115452476934E-17, 0.000000000000000000 ) ) ;
#13399 = CARTESIAN_POINT ( 'NONE',  ( -1.500000000000000000, 9.886859966642591147, 150.0000000000000284 ) ) ;
#13400 = ORIENTED_EDGE ( 'NONE', *, *, #22, .F. ) ;
#13401 = ORIENTED_EDGE ( 'NONE', *, *, #16613, .F. ) ;
#13402 = CARTESIAN_POINT ( 'NONE',  ( 0.000000000000000000, 0.000000000000000000, -100.0000000000000000 ) ) ;
#13403 = DIRECTION ( 'NONE',  ( -1.000000000000000000, 0.000000000000000000, -0.000000000000000000 ) ) ;
#13404 = AXIS2_PLACEMENT_3D ( 'NONE', #1792, #3254, #12847 ) ;
#13405 = FACE_BOUND ( 'NONE', #18508, .T. ) ;
#13406 = EDGE_LOOP ( 'NONE', ( #18963, #12585 ) ) ;
#13407 = FACE_OUTER_BOUND ( 'NONE', #4342, .T. ) ;
#13408 = FACE_OUTER_BOUND ( 'NONE', #3527, .T. ) ;
#13409 = DIRECTION ( 'NONE',  ( -0.000000000000000000, -0.000000000000000000, 1.000000000000000000 ) ) ;
#13410 = VERTEX_POINT ( 'NONE', #5479 ) ;
#13411 = FACE_OUTER_BOUND ( 'NONE', #16900, .T. ) ;
#13412 = CARTESIAN_POINT ( 'NONE',  ( 2.500000000000000000, -1.768423874527823125, 1.021000000000002128 ) ) ;
#13413 = CARTESIAN_POINT ( 'NONE',  ( 0.000000000000000000, 0.000000000000000000, 4.000000000000000000 ) ) ;
#13414 = ORIENTED_EDGE ( 'NONE', *, *, #9929, .F. ) ;
#13415 = ADVANCED_FACE ( 'NONE', ( #18613 ), #12888, .T. ) ;
#13416 = DIRECTION ( 'NONE',  ( 1.000000000000000000, -0.000000000000000000, 6.982962677686266711E-15 ) ) ;
#13417 = CONTEXT_DEPENDENT_SHAPE_REPRESENTATION ( #14068, #19811 ) ;
#13418 = DIRECTION ( 'NONE',  ( 0.000000000000000000, -1.000000000000000000, 0.000000000000000000 ) ) ;
#13419 = PLANE ( 'NONE',  #8049 ) ;
#13420 = DIRECTION ( 'NONE',  ( 0.000000000000000000, 0.000000000000000000, 1.000000000000000000 ) ) ;
#13421 = EDGE_CURVE ( 'NONE', #5237, #5249, #165, .T. ) ;
#13422 = EDGE_CURVE ( 'NONE', #2021, #8380, #18654, .T. ) ;
#13423 = VERTEX_POINT ( 'NONE', #18515 ) ;
#13424 = ORIENTED_EDGE ( 'NONE', *, *, #16963, .T. ) ;
#13425 = CARTESIAN_POINT ( 'NONE',  ( 2.500000000000000000, 0.000000000000000000, 0.000000000000000000 ) ) ;
#13426 = FACE_OUTER_BOUND ( 'NONE', #3682, .T. ) ;
#13427 = AXIS2_PLACEMENT_3D ( 'NONE', #11247, #3585, #1896 ) ;
#13428 = ADVANCED_FACE ( 'NONE', ( #5712 ), #9470, .F. ) ;
#13429 = CIRCLE ( 'NONE', #291, 2.649999999999971934 ) ;
#13430 =( REPRESENTATION_RELATIONSHIP ('NONE','NONE', #10127, #5587 ) REPRESENTATION_RELATIONSHIP_WITH_TRANSFORMATION ( #17804 )SHAPE_REPRESENTATION_RELATIONSHIP( ) );
#13431 = ORIENTED_EDGE ( 'NONE', *, *, #20489, .T. ) ;
#13432 = DIRECTION ( 'NONE',  ( 1.000000000000000000, -6.938893903907227392E-16, 2.425604463963772562E-30 ) ) ;
#13433 = CARTESIAN_POINT ( 'NONE',  ( 17.00000000000000000, 0.000000000000000000, 0.000000000000000000 ) ) ;
#13434 = VERTEX_POINT ( 'NONE', #13005 ) ;
#13435 = CIRCLE ( 'NONE', #12280, 2.649999999999985700 ) ;
#13436 = LINE ( 'NONE', #10271, #10640 ) ;
#13437 = AXIS2_PLACEMENT_3D ( 'NONE', #2048, #11650, #5820 ) ;
#13438 = VERTEX_POINT ( 'NONE', #22486 ) ;
#13439 =( NAMED_UNIT ( * ) PLANE_ANGLE_UNIT ( ) SI_UNIT ( $, .RADIAN. ) );
#13440 = LINE ( 'NONE', #17035, #20555 ) ;
#13441 = ORIENTED_EDGE ( 'NONE', *, *, #6670, .F. ) ;
#13442 = EDGE_LOOP ( 'NONE', ( #15738, #12920, #9049, #5233 ) ) ;
#13443 = PLANE ( 'NONE',  #11207 ) ;
#13444 = FACE_OUTER_BOUND ( 'NONE', #15154, .T. ) ;
#13445 = CARTESIAN_POINT ( 'NONE',  ( -21.69904058246455847, -1012.523990643698880, -145.0000000000001421 ) ) ;
#13446 = VECTOR ( 'NONE', #10118, 1000.000000000000114 ) ;
#13447 = CARTESIAN_POINT ( 'NONE',  ( 285.1999999999999318, 267.7999999999999545, 146.4928932188134922 ) ) ;
#13448 = DIRECTION ( 'NONE',  ( 5.618537574013950123E-17, 3.483493295888648978E-15, 1.000000000000000000 ) ) ;
#13449 = B_SPLINE_CURVE_WITH_KNOTS ( 'NONE', 3,
 ( #2425, #11167, #14891, #6050, #13466, #13230, #7621, #18962, #9814, #11521, #20537, #1953, #9341, #150, #22225, #5696, #11401, #3882, #18601, #18717, #2177, #17055, #9566, #16931, #5936, #17169, #401, #7760 ),
 .UNSPECIFIED., .F., .F.,
 ( 4, 2, 2, 2, 2, 2, 2, 2, 2, 2, 2, 2, 2, 4 ),
 ( 0.007862850516741886481, 0.008354729399060628267, 0.008846608281379370053, 0.009830366046016853626, 0.01032224492833538204, 0.01081412381065390872, 0.01130600269297243540, 0.01179788157529096382, 0.01278163933992802759, 0.01327351822224656294, 0.01376539710456510177, 0.01425727598688363712, 0.01474915486920217247, 0.01573291263383924665 ),
 .UNSPECIFIED. ) ;
#13450 = DIRECTION ( 'NONE',  ( 0.000000000000000000, 0.000000000000000000, -1.000000000000000000 ) ) ;
#13451 = EDGE_CURVE ( 'NONE', #1796, #21139, #18382, .T. ) ;
#13452 = CARTESIAN_POINT ( 'NONE',  ( -145.0000000000000284, -5.062647941322544249E-13, -90.00000000000000000 ) ) ;
#13453 = VERTEX_POINT ( 'NONE', #9353 ) ;
#13454 = EDGE_CURVE ( 'NONE', #10574, #12356, #2079, .T. ) ;
#13455 = PLANE ( 'NONE',  #13437 ) ;
#13456 = VECTOR ( 'NONE', #12521, 1000.000000000000000 ) ;
#13457 = CYLINDRICAL_SURFACE ( 'NONE', #18372, 2.649999999999971934 ) ;
#13458 = SHAPE_REPRESENTATION_RELATIONSHIP ( 'NONE' , 'NONE' ,  #9771, #9029 ) ;
#13459 = AXIS2_PLACEMENT_3D ( 'NONE', #8524, #16121, #14338 ) ;
#13460 = CIRCLE ( 'NONE', #18414, 9.999999999999998224 ) ;
#13461 = VERTEX_POINT ( 'NONE', #2080 ) ;
#13462 = CARTESIAN_POINT ( 'NONE',  ( -136.1788113199118584, -1074.029417785592386, -32.37389708099358643 ) ) ;
#13463 = CARTESIAN_POINT ( 'NONE',  ( 280.6220388411722411, 271.9822575857425022, -148.2140793454687469 ) ) ;
#13464 = ADVANCED_FACE ( 'NONE', ( #2328 ), #3795, .T. ) ;
#13465 = EDGE_LOOP ( 'NONE', ( #13100, #22217 ) ) ;
#13466 = CARTESIAN_POINT ( 'NONE',  ( -135.3962747006860354, -1075.451122483741756, 32.37380477188061434 ) ) ;
#13467 = ORIENTED_EDGE ( 'NONE', *, *, #10189, .F. ) ;
#13468 = CARTESIAN_POINT ( 'NONE',  ( -109.8074641843669781, -85.22886158240918064, -90.00000000000000000 ) ) ;
#13469 = CIRCLE ( 'NONE', #6100, 145.0000000000000284 ) ;
#13470 = DIRECTION ( 'NONE',  ( -0.000000000000000000, 1.000000000000000000, -3.469446951953613794E-15 ) ) ;
#13471 = ORIENTED_EDGE ( 'NONE', *, *, #2973, .F. ) ;
#13472 = EDGE_CURVE ( 'NONE', #18851, #7954, #4127, .T. ) ;
#13473 = AXIS2_PLACEMENT_3D ( 'NONE', #10796, #18139, #1587 ) ;
#13474 = CARTESIAN_POINT ( 'NONE',  ( 51.87806360044912424, -135.4018704341552279, -2.775557561562891351E-14 ) ) ;
#13475 = AXIS2_PLACEMENT_3D ( 'NONE', #4675, #12088, #12802 ) ;
#13476 = PRESENTATION_STYLE_ASSIGNMENT (( #2068 ) ) ;
#13477 = AXIS2_PLACEMENT_3D ( 'NONE', #11358, #22544, #18673 ) ;
#13478 = CONTEXT_DEPENDENT_SHAPE_REPRESENTATION ( #4944, #15327 ) ;
#13479 = ORIENTED_EDGE ( 'NONE', *, *, #7745, .F. ) ;
#13480 = CARTESIAN_POINT ( 'NONE',  ( 0.000000000000000000, 0.000000000000000000, -100.0000000000000000 ) ) ;
#13481 = EDGE_LOOP ( 'NONE', ( #13081, #1055, #5145, #4820 ) ) ;
#13482 = CARTESIAN_POINT ( 'NONE',  ( -23.72531794788157100, -991.9499648419341611, -145.0000000000001421 ) ) ;
#13483 = CARTESIAN_POINT ( 'NONE',  ( 3.749999999999998224, 6.495190528383290918, -6.991905250253753756 ) ) ;
#13484 = CARTESIAN_POINT ( 'NONE',  ( 45.00000000000000000, 272.9999999999999432, -5.249999999999991118 ) ) ;
#13485 = CARTESIAN_POINT ( 'NONE',  ( 7.499999999999999112, 41.99999999999998579, 100.0000000000000000 ) ) ;
#13486 = ORIENTED_EDGE ( 'NONE', *, *, #7396, .T. ) ;
#13487 = CARTESIAN_POINT ( 'NONE',  ( -282.2000000000000455, 267.9452901038201276, 146.4301275412297230 ) ) ;
#13489 = ORIENTED_EDGE ( 'NONE', *, *, #20501, .T. ) ;
#13488 = ORIENTED_EDGE ( 'NONE', *, *, #1025, .T. ) ;
#13490 = AXIS2_PLACEMENT_3D ( 'NONE', #15919, #10500, #19389 ) ;
#13491 = CARTESIAN_POINT ( 'NONE',  ( 142.1569981022717286, 83.57863297847661954, -29.99999999999344880 ) ) ;
#13492 = EDGE_CURVE ( 'NONE', #8328, #19306, #16467, .T. ) ;
#13493 = VECTOR ( 'NONE', #10870, 1000.000000000000000 ) ;
#13494 = CARTESIAN_POINT ( 'NONE',  ( -102.3500000000000369, 30.00000000000001421, 3.000000000000000000 ) ) ;
#13495 = CARTESIAN_POINT ( 'NONE',  ( -35.00000000000000000, 0.000000000000000000, 100.0000000000000000 ) ) ;
#13496 = EDGE_CURVE ( 'NONE', #19782, #16311, #978, .T. ) ;
#13497 = AXIS2_PLACEMENT_3D ( 'NONE', #7952, #6138, #13906 ) ;
#13498 = EDGE_CURVE ( 'NONE', #20268, #11652, #8359, .T. ) ;
#13499 = CARTESIAN_POINT ( 'NONE',  ( 279.9999999999999432, 269.9696999999999889, 145.0000000000000284 ) ) ;
#13500 = FACE_BOUND ( 'NONE', #13373, .T. ) ;
#13501 = EDGE_CURVE ( 'NONE', #11863, #13198, #18453, .T. ) ;
#13502 = VERTEX_POINT ( 'NONE', #13485 ) ;
#13503 = VECTOR ( 'NONE', #22424, 1000.000000000000114 ) ;
#13504 = CARTESIAN_POINT ( 'NONE',  ( 90.00000000000000000, 3.000000000000293987, 129.9038105676659711 ) ) ;
#13505 = EDGE_CURVE ( 'NONE', #23227, #22100, #4574, .T. ) ;
#13506 = LINE ( 'NONE', #433, #13789 ) ;
#13507 = EDGE_CURVE ( 'NONE', #2833, #21387, #12042, .T. ) ;
#13508 = CARTESIAN_POINT ( 'NONE',  ( 123.8018707182401101, -1093.263712923000639, 32.24990070396069086 ) ) ;
#13509 = VERTEX_POINT ( 'NONE', #2560 ) ;
#13510 = DIRECTION ( 'NONE',  ( 1.000000000000000000, 0.000000000000000000, 0.000000000000000000 ) ) ;
#13511 = ORIENTED_EDGE ( 'NONE', *, *, #9781, .T. ) ;
#13513 = LINE ( 'NONE', #22762, #8716 ) ;
#13512 = AXIS2_PLACEMENT_3D ( 'NONE', #20949, #5860, #5746 ) ;
#13514 = CARTESIAN_POINT ( 'NONE',  ( 279.9999999999999432, 272.9999999999999432, -144.9999999999999716 ) ) ;
#13516 = VECTOR ( 'NONE', #12429, 1000.000000000000000 ) ;
#13515 =( GEOMETRIC_REPRESENTATION_CONTEXT ( 3 ) GLOBAL_UNCERTAINTY_ASSIGNED_CONTEXT ( ( #20264 ) ) GLOBAL_UNIT_ASSIGNED_CONTEXT ( ( #18227, #21841, #23554 ) ) REPRESENTATION_CONTEXT ( 'NONE', 'WORKASPACE' ) );
#13517 = ORIENTED_EDGE ( 'NONE', *, *, #23493, .F. ) ;
#13518 = VECTOR ( 'NONE', #2357, 1000.000000000000114 ) ;
#13519 = CARTESIAN_POINT ( 'NONE',  ( 15.25457574233253055, 19.87452195056642168, -145.0000000000000000 ) ) ;
#13520 = AXIS2_PLACEMENT_3D ( 'NONE', #448, #17354, #4411 ) ;
#13521 = ORIENTED_EDGE ( 'NONE', *, *, #13297, .F. ) ;
#13522 = CARTESIAN_POINT ( 'NONE',  ( -24.99999999999996092, -37.41657386773943728, 65.00000000000012790 ) ) ;
#13523 = CONICAL_SURFACE ( 'NONE', #21575, 2.041999999999999815, 1.047197551196591858 ) ;
#13524 = DIRECTION ( 'NONE',  ( 1.302872740555339390E-32, -4.694093751100962712E-16, 1.000000000000000000 ) ) ;
#13525 = CARTESIAN_POINT ( 'NONE',  ( 2.500000000000000000, 0.000000000000000000, 0.000000000000000000 ) ) ;
#13526 = DIRECTION ( 'NONE',  ( 0.5877852522924719159, 0.8090169943749482284, 0.000000000000000000 ) ) ;
#13527 = FACE_OUTER_BOUND ( 'NONE', #12635, .T. ) ;
#13528 = FACE_OUTER_BOUND ( 'NONE', #11240, .T. ) ;
#13529 = DIRECTION ( 'NONE',  ( -1.000000000000000000, 0.000000000000000000, 0.000000000000000000 ) ) ;
#13530 = ORIENTED_EDGE ( 'NONE', *, *, #19048, .T. ) ;
#13531 = CARTESIAN_POINT ( 'NONE',  ( 100.0000000000000000, 249.9999999999999716, 145.0000000000000284 ) ) ;
#13532 = DIRECTION ( 'NONE',  ( 0.000000000000000000, 0.000000000000000000, 1.000000000000000000 ) ) ;
#13533 = ORIENTED_EDGE ( 'NONE', *, *, #18176, .F. ) ;
#13534 = VERTEX_POINT ( 'NONE', #757 ) ;
#13535 = CARTESIAN_POINT ( 'NONE',  ( -31.74999999999995737, 0.000000000000000000, 0.000000000000000000 ) ) ;
#13536 = DIRECTION ( 'NONE',  ( 0.000000000000000000, 0.000000000000000000, 1.000000000000000000 ) ) ;
#13537 = AXIS2_PLACEMENT_3D ( 'NONE', #15874, #14072, #23207 ) ;
#13538 =( GEOMETRIC_REPRESENTATION_CONTEXT ( 3 ) GLOBAL_UNCERTAINTY_ASSIGNED_CONTEXT ( ( #6007 ) ) GLOBAL_UNIT_ASSIGNED_CONTEXT ( ( #12146, #17650, #2050 ) ) REPRESENTATION_CONTEXT ( 'NONE', 'WORKASPACE' ) );
#13539 = CIRCLE ( 'NONE', #19652, 2.500000000000000444 ) ;
#13540 = AXIS2_PLACEMENT_3D ( 'NONE', #3263, #8721, #1454 ) ;
#13541 = PLANE ( 'NONE',  #9068 ) ;
#13542 = VECTOR ( 'NONE', #8028, 1000.000000000000000 ) ;
#13543 = AXIS2_PLACEMENT_3D ( 'NONE', #8800, #12922, #8930 ) ;
#13544 = VERTEX_POINT ( 'NONE', #20919 ) ;
#13545 = EDGE_CURVE ( 'NONE', #20480, #10816, #13836, .T. ) ;
#13546 = CARTESIAN_POINT ( 'NONE',  ( 126.3653543294811499, 77.28387428943223370, 27.94500000000641649 ) ) ;
#13547 = EDGE_CURVE ( 'NONE', #18184, #8675, #8443, .T. ) ;
#13548 = DIRECTION ( 'NONE',  ( 0.000000000000000000, -0.5000000000000009992, -0.8660254037844380415 ) ) ;
#13549 = DIRECTION ( 'NONE',  ( -0.000000000000000000, -0.000000000000000000, 1.000000000000000000 ) ) ;
#13550 = VERTEX_POINT ( 'NONE', #528 ) ;
#13551 = CARTESIAN_POINT ( 'NONE',  ( 16.55500000000001393, 0.000000000000000000, 2.500000000000000444 ) ) ;
#13552 = DIRECTION ( 'NONE',  ( 1.000000000000000000, 0.000000000000000000, 0.000000000000000000 ) ) ;
#13553 = UNCERTAINTY_MEASURE_WITH_UNIT (LENGTH_MEASURE( 1.000000000000000082E-05 ), #9334, 'distance_accuracy_value', 'NONE');
#13554 = CARTESIAN_POINT ( 'NONE',  ( 2.500000000000000000, 2.357898499370432166, -2.385244779468109755E-15 ) ) ;
#13555 = VERTEX_POINT ( 'NONE', #10086 ) ;
#13556 = CARTESIAN_POINT ( 'NONE',  ( 70.00000000000000000, -87.33333333333332860, 145.0000000000000000 ) ) ;
#13557 = CONTEXT_DEPENDENT_SHAPE_REPRESENTATION ( #17544, #5167 ) ;
#13558 = CARTESIAN_POINT ( 'NONE',  ( 0.000000000000000000, 0.000000000000000000, -4.974599999999998801 ) ) ;
#13559 = AXIS2_PLACEMENT_3D ( 'NONE', #17987, #6874, #3358 ) ;
#13560 = CIRCLE ( 'NONE', #21976, 2.200000000000028155 ) ;
#13562 = DIRECTION ( 'NONE',  ( 1.000000000000000000, 0.000000000000000000, 0.000000000000000000 ) ) ;
#13561 = PRESENTATION_LAYER_ASSIGNMENT (  '', '', ( #6557 ) ) ;
#13563 = VECTOR ( 'NONE', #5824, 1000.000000000000114 ) ;
#13564 = CYLINDRICAL_SURFACE ( 'NONE', #22462, 2.649999999999999467 ) ;
#13565 = AXIS2_PLACEMENT_3D ( 'NONE', #20028, #3490, #14853 ) ;
#13566 = AXIS2_PLACEMENT_3D ( 'NONE', #3775, #9722, #6077 ) ;
#13567 = ORIENTED_EDGE ( 'NONE', *, *, #2476, .F. ) ;
#13568 = ORIENTED_EDGE ( 'NONE', *, *, #11176, .F. ) ;
#13569 = CARTESIAN_POINT ( 'NONE',  ( 19.87769063953886928, -15.24974479720507148, 145.0000119999999981 ) ) ;
#13570 = CARTESIAN_POINT ( 'NONE',  ( 10.00000000000000178, 0.000000000000000000, 8.000000000000000000 ) ) ;
#13571 = ORIENTED_EDGE ( 'NONE', *, *, #19305, .T. ) ;
#13572 = LINE ( 'NONE', #3956, #5189 ) ;
#13573 = CARTESIAN_POINT ( 'NONE',  ( -127.1852154257921086, 88.59424271557165298, 27.82653936295257324 ) ) ;
#13574 = AXIS2_PLACEMENT_3D ( 'NONE', #3487, #1900, #20026 ) ;
#13575 = ORIENTED_EDGE ( 'NONE', *, *, #5297, .F. ) ;
#13576 = DIRECTION ( 'NONE',  ( 1.000000000000000000, 0.000000000000000000, 0.000000000000000000 ) ) ;
#13577 = ORIENTED_EDGE ( 'NONE', *, *, #12730, .F. ) ;
#13578 =( LENGTH_UNIT ( ) NAMED_UNIT ( * ) SI_UNIT ( .MILLI., .METRE. ) );
#13579 = DIRECTION ( 'NONE',  ( 1.000000000000000000, 0.000000000000000000, 0.000000000000000000 ) ) ;
#13580 = VERTEX_POINT ( 'NONE', #13609 ) ;
#13581 = ORIENTED_EDGE ( 'NONE', *, *, #594, .F. ) ;
#13582 = LINE ( 'NONE', #13806, #6535 ) ;
#13583 = PRODUCT_DEFINITION_SHAPE ( 'NONE', 'NONE',  #23863 ) ;
#13584 = CARTESIAN_POINT ( 'NONE',  ( 0.000000000000000000, 0.000000000000000000, -150.0000000000000000 ) ) ;
#13585 = PLANE ( 'NONE',  #18448 ) ;
#13586 = CARTESIAN_POINT ( 'NONE',  ( 45.00000000000004974, -52.79999999999965610, 105.0000000000001990 ) ) ;
#13587 = CYLINDRICAL_SURFACE ( 'NONE', #7292, 7.500000000000007105 ) ;
#13588 = ORIENTED_EDGE ( 'NONE', *, *, #23484, .T. ) ;
#13589 = CYLINDRICAL_SURFACE ( 'NONE', #7590, 2.500000000000000444 ) ;
#13590 = APPLICATION_CONTEXT ( 'automotive_design' ) ;
#13591 = VERTEX_POINT ( 'NONE', #17426 ) ;
#13592 = DIRECTION ( 'NONE',  ( 0.000000000000000000, 0.000000000000000000, -1.000000000000000000 ) ) ;
#13593 = DIRECTION ( 'NONE',  ( 0.000000000000000000, 1.000000000000000000, 0.000000000000000000 ) ) ;
#13594 = ORIENTED_EDGE ( 'NONE', *, *, #10067, .T. ) ;
#13595 = CARTESIAN_POINT ( 'NONE',  ( -11.08405391225051595, -22.46867509500516036, -145.0000000000000000 ) ) ;
#13596 = ORIENTED_EDGE ( 'NONE', *, *, #14506, .T. ) ;
#13597 = CARTESIAN_POINT ( 'NONE',  ( -79.99999999999995737, -138.0000000000000284, 3.000000000000000000 ) ) ;
#13598 = CARTESIAN_POINT ( 'NONE',  ( 0.000000000000000000, 0.000000000000000000, 100.0000000000000000 ) ) ;
#13599 = VERTEX_POINT ( 'NONE', #15624 ) ;
#13600 = EDGE_CURVE ( 'NONE', #21974, #5229, #21554, .T. ) ;
#13601 = CARTESIAN_POINT ( 'NONE',  ( -40.33333333333332860, -89.99999999999997158, 3.000000000000000000 ) ) ;
#13602 = ADVANCED_FACE ( 'NONE', ( #23078 ), #4377, .F. ) ;
#13603 = EDGE_CURVE ( 'NONE', #12326, #14560, #19098, .T. ) ;
#13604 = ORIENTED_EDGE ( 'NONE', *, *, #12076, .T. ) ;
#13605 = CARTESIAN_POINT ( 'NONE',  ( 45.24999999999994316, 100.0000000000000000, 145.0000000000000000 ) ) ;
#13606 = CARTESIAN_POINT ( 'NONE',  ( -100.0000000000001137, -132.1999999999999602, 177.2000000000014097 ) ) ;
#13607 = EDGE_CURVE ( 'NONE', #11805, #19135, #17310, .T. ) ;
#13608 = CARTESIAN_POINT ( 'NONE',  ( 79.04925354955072692, 121.5574576620408322, -2.775557561562891351E-14 ) ) ;
#13609 = CARTESIAN_POINT ( 'NONE',  ( -10.00000000000000000, 1.224646799147353256E-15, 20.00000000000000000 ) ) ;
#13610 = ORIENTED_EDGE ( 'NONE', *, *, #13208, .T. ) ;
#13611 = CARTESIAN_POINT ( 'NONE',  ( -281.3684637172358975, 268.4847249064868038, -150.2299999999999613 ) ) ;
#13612 =( NAMED_UNIT ( * ) SI_UNIT ( $, .STERADIAN. ) SOLID_ANGLE_UNIT ( ) );
#13614 = ORIENTED_EDGE ( 'NONE', *, *, #18745, .F. ) ;
#13613 = ORIENTED_EDGE ( 'NONE', *, *, #3938, .T. ) ;
#13615 = CARTESIAN_POINT ( 'NONE',  ( 131.4546237677518548, -1099.567474056937272, -29.99999999999344880 ) ) ;
#13616 = CARTESIAN_POINT ( 'NONE',  ( -7.549004593702462351, -4.358419834287841965, -7.700121441565841884 ) ) ;
#13617 = CARTESIAN_POINT ( 'NONE',  ( 90.00000000000000000, 76.26794919243113213, 3.000000000000002665 ) ) ;
#13618 = CARTESIAN_POINT ( 'NONE',  ( 284.1822575857424340, 271.0140793454687582, 145.8708543776411943 ) ) ;
#13619 = CARTESIAN_POINT ( 'NONE',  ( -283.2140793454688605, 271.9822575857424454, -145.6220388411722411 ) ) ;
#13620 = ORIENTED_EDGE ( 'NONE', *, *, #1857, .F. ) ;
#13621 = CARTESIAN_POINT ( 'NONE',  ( -51.87806360044718446, -135.4018704341559953, 90.00000000000000000 ) ) ;
#13622 = DIRECTION ( 'NONE',  ( -0.000000000000000000, 1.000000000000000000, -0.000000000000000000 ) ) ;
#13623 =( REPRESENTATION_RELATIONSHIP ('NONE','NONE', #10127, #11474 ) REPRESENTATION_RELATIONSHIP_WITH_TRANSFORMATION ( #1365 )SHAPE_REPRESENTATION_RELATIONSHIP( ) );
#13624 = CARTESIAN_POINT ( 'NONE',  ( 122.9459112154328579, -1094.389103796012705, 30.16266818053248500 ) ) ;
#13625 = CONTEXT_DEPENDENT_SHAPE_REPRESENTATION ( #18318, #10683 ) ;
#13626 = ORIENTED_EDGE ( 'NONE', *, *, #22720, .T. ) ;
#13627 = AXIS2_PLACEMENT_3D ( 'NONE', #574, #15200, #8299 ) ;
#13628 = LINE ( 'NONE', #11564, #22139 ) ;
#13629 = EDGE_CURVE ( 'NONE', #12485, #18619, #7648, .T. ) ;
#13630 = VERTEX_POINT ( 'NONE', #22602 ) ;
#13631 = DIRECTION ( 'NONE',  ( -0.9423651898111408132, -0.3345860861306287348, 6.982962677686266711E-15 ) ) ;
#13632 = DIRECTION ( 'NONE',  ( 0.000000000000000000, 0.000000000000000000, 1.000000000000000000 ) ) ;
#13633 = ORIENTED_EDGE ( 'NONE', *, *, #19488, .F. ) ;
#13634 = CARTESIAN_POINT ( 'NONE',  ( 3.266776071704960316, 24.83992656739923177, -145.0000000000000000 ) ) ;
#13635 = ADVANCED_FACE ( 'NONE', ( #867 ), #20801, .F. ) ;
#13636 = VERTEX_POINT ( 'NONE', #4267 ) ;
#13637 = DIRECTION ( 'NONE',  ( -0.000000000000000000, 1.000000000000000000, 0.000000000000000000 ) ) ;
#13638 = CARTESIAN_POINT ( 'NONE',  ( 0.000000000000000000, 0.000000000000000000, 65.00000000000000000 ) ) ;
#13639 = EDGE_CURVE ( 'NONE', #19785, #14374, #639, .T. ) ;
#13640 = CARTESIAN_POINT ( 'NONE',  ( -135.4018704341554269, -51.87806360044866238, -2.775557561562891351E-14 ) ) ;
#13641 = DIRECTION ( 'NONE',  ( -0.8660254037844373753, 0.5000000000000021094, 0.000000000000000000 ) ) ;
#13642 = CARTESIAN_POINT ( 'NONE',  ( 5.000000000000002665, 3.306546357697854226E-16, 2.700000000000000622 ) ) ;
#13643 = PLANE ( 'NONE',  #11596 ) ;
#13644 = CARTESIAN_POINT ( 'NONE',  ( 5.000000000000000000, -2.342598717236900718, 4.057500000000001883 ) ) ;
#13645 = EDGE_CURVE ( 'NONE', #1257, #18998, #15001, .T. ) ;
#13646 = ORIENTED_EDGE ( 'NONE', *, *, #9316, .F. ) ;
#13647 = SURFACE_STYLE_FILL_AREA ( #23123 ) ;
#13648 = DIRECTION ( 'NONE',  ( 0.000000000000000000, 0.000000000000000000, 1.000000000000000000 ) ) ;
#13649 = CARTESIAN_POINT ( 'NONE',  ( -40.00000000000000000, 100.0000000000000000, 150.2000000000009550 ) ) ;
#13650 = ORIENTED_EDGE ( 'NONE', *, *, #2777, .F. ) ;
#13651 = CIRCLE ( 'NONE', #866, 4.250000000000000000 ) ;
#13652 = ORIENTED_EDGE ( 'NONE', *, *, #1199, .T. ) ;
#13653 = DIRECTION ( 'NONE',  ( 1.000000000000000000, 3.736327486719275871E-16, -1.296299001029869881E-30 ) ) ;
#13654 = CARTESIAN_POINT ( 'NONE',  ( -281.4928932188135491, -129.2000000000000455, 177.2000000000014097 ) ) ;
#13655 = FACE_OUTER_BOUND ( 'NONE', #9879, .T. ) ;
#13656 = ORIENTED_EDGE ( 'NONE', *, *, #11541, .F. ) ;
#13657 = CARTESIAN_POINT ( 'NONE',  ( -79.99999999999997158, -62.00000000000001421, 5.199999999999997513 ) ) ;
#13658 = DIRECTION ( 'NONE',  ( -0.000000000000000000, 1.000000000000000000, -0.000000000000000000 ) ) ;
#13659 = CARTESIAN_POINT ( 'NONE',  ( -3.355112389629170799, 2.681727112203152963, -0.2256878752776689534 ) ) ;
#13660 = ORIENTED_EDGE ( 'NONE', *, *, #2170, .F. ) ;
#13661 = CARTESIAN_POINT ( 'NONE',  ( 281.4301685938040691, 268.1431883596741841, 150.1999999999999602 ) ) ;
#13662 = PLANE ( 'NONE',  #23138 ) ;
#13663 = PRESENTATION_STYLE_ASSIGNMENT (( #2500 ) ) ;
#13664 = VERTEX_POINT ( 'NONE', #13719 ) ;
#13665 = CARTESIAN_POINT ( 'NONE',  ( 282.1696999999999775, 268.0840560642351988, -146.3684665762323789 ) ) ;
#13666 = VECTOR ( 'NONE', #6706, 1000.000000000000000 ) ;
#13667 = CONTEXT_DEPENDENT_SHAPE_REPRESENTATION ( #6637, #21258 ) ;
#13668 = DIRECTION ( 'NONE',  ( -1.000000000000000000, -4.183096374613631247E-18, 0.000000000000000000 ) ) ;
#13669 = DIRECTION ( 'NONE',  ( 6.982962677686266711E-15, -9.837870180509810443E-29, 1.000000000000000000 ) ) ;
#13670 = DIRECTION ( 'NONE',  ( 0.000000000000000000, 0.000000000000000000, 1.000000000000000000 ) ) ;
#13671 = ORIENTED_EDGE ( 'NONE', *, *, #18205, .F. ) ;
#13673 = VERTEX_POINT ( 'NONE', #6906 ) ;
#13672 = EDGE_CURVE ( 'NONE', #22100, #23227, #15400, .T. ) ;
#13674 = EDGE_CURVE ( 'NONE', #20911, #4011, #7267, .T. ) ;
#13675 = CARTESIAN_POINT ( 'NONE',  ( -45.00000000000000000, 272.9999999999999432, 0.000000000000000000 ) ) ;
#13676 = CYLINDRICAL_SURFACE ( 'NONE', #9076, 7.500000000000007105 ) ;
#13677 = EDGE_CURVE ( 'NONE', #3139, #7964, #3154, .T. ) ;
#13678 = AXIS2_PLACEMENT_3D ( 'NONE', #2438, #11904, #19211 ) ;
#13679 = AXIS2_PLACEMENT_3D ( 'NONE', #12335, #17483, #928 ) ;
#13680 = ORIENTED_EDGE ( 'NONE', *, *, #7243, .T. ) ;
#13681 = DIRECTION ( 'NONE',  ( -1.000000000000000000, -0.000000000000000000, -0.000000000000000000 ) ) ;
#13682 = CARTESIAN_POINT ( 'NONE',  ( -127.1840658299263112, 88.59589253999637037, 32.17229779615544771 ) ) ;
#13683 = EDGE_LOOP ( 'NONE', ( #7585, #22369, #7722, #4700 ) ) ;
#13684 = LINE ( 'NONE', #21003, #13736 ) ;
#13685 = ORIENTED_EDGE ( 'NONE', *, *, #4902, .F. ) ;
#13686 = CARTESIAN_POINT ( 'NONE',  ( -4.024497503033519941, -2.323544716729390558, -3.572167766733381544 ) ) ;
#13687 = FACE_OUTER_BOUND ( 'NONE', #12308, .T. ) ;
#13688 = ORIENTED_EDGE ( 'NONE', *, *, #13545, .F. ) ;
#13689 = ORIENTED_EDGE ( 'NONE', *, *, #14394, .F. ) ;
#13690 = CARTESIAN_POINT ( 'NONE',  ( 4.211140560182196957, 2.431303136016536470, -3.745885042887433514 ) ) ;
#13691 = AXIS2_PLACEMENT_3D ( 'NONE', #14848, #22179, #13191 ) ;
#13692 = CARTESIAN_POINT ( 'NONE',  ( -91.18044947428876412, -112.7436279071535239, 90.00000000000000000 ) ) ;
#13693 = CIRCLE ( 'NONE', #3221, 5.249999999999949374 ) ;
#13694 = DIRECTION ( 'NONE',  ( 0.000000000000000000, -0.000000000000000000, 1.000000000000000000 ) ) ;
#13695 = DIRECTION ( 'NONE',  ( 0.000000000000000000, 1.000000000000000000, -5.286776307738891306E-15 ) ) ;
#13696 = ORIENTED_EDGE ( 'NONE', *, *, #14394, .T. ) ;
#13697 = EDGE_CURVE ( 'NONE', #15272, #931, #17323, .T. ) ;
#13698 = CARTESIAN_POINT ( 'NONE',  ( 2.500000000000002220, 2.357898499370434386, -3.469446951953614189E-15 ) ) ;
#13699 =( NAMED_UNIT ( * ) PLANE_ANGLE_UNIT ( ) SI_UNIT ( $, .RADIAN. ) );
#13700 = ORIENTED_EDGE ( 'NONE', *, *, #8789, .T. ) ;
#13701 = EDGE_CURVE ( 'NONE', #10033, #21432, #8840, .T. ) ;
#13702 = CARTESIAN_POINT ( 'NONE',  ( 2.449848172108560096, 3.432307619358740514, -3.503702292528905637 ) ) ;
#13703 = ORIENTED_EDGE ( 'NONE', *, *, #21629, .T. ) ;
#13704 = LINE ( 'NONE', #17512, #16081 ) ;
#13705 = VECTOR ( 'NONE', #16122, 1000.000000000000000 ) ;
#13706 = EDGE_LOOP ( 'NONE', ( #20156, #22482, #19183, #14398 ) ) ;
#13707 = CARTESIAN_POINT ( 'NONE',  ( 20.00000000000000000, 0.000000000000000000, -150.0000000000000000 ) ) ;
#13708 = AXIS2_PLACEMENT_3D ( 'NONE', #14510, #7469, #1919 ) ;
#13709 = FACE_OUTER_BOUND ( 'NONE', #23322, .T. ) ;
#13710 = ORIENTED_EDGE ( 'NONE', *, *, #20938, .T. ) ;
#13711 = CARTESIAN_POINT ( 'NONE',  ( -280.9952621458756994, 270.4188186979286002, 149.5436892194421716 ) ) ;
#13712 = CARTESIAN_POINT ( 'NONE',  ( 52.00000000000000711, -62.00000000000001421, -3.122502256758252770E-14 ) ) ;
#13713 = EDGE_LOOP ( 'NONE', ( #19277, #2821, #19556, #16026 ) ) ;
#13714 = PLANE ( 'NONE',  #6010 ) ;
#13715 = AXIS2_PLACEMENT_3D ( 'NONE', #4752, #8511, #15887 ) ;
#13716 = CARTESIAN_POINT ( 'NONE',  ( -67.34999999999996589, -87.33333333333338544, 0.000000000000000000 ) ) ;
#13717 = EDGE_CURVE ( 'NONE', #11975, #15717, #5332, .T. ) ;
#13718 = AXIS2_PLACEMENT_3D ( 'NONE', #11690, #8381, #17917 ) ;
#13719 = CARTESIAN_POINT ( 'NONE',  ( 7.499999999999997335, 34.18698582794336005, -100.0000000000000000 ) ) ;
#13720 = EDGE_LOOP ( 'NONE', ( #13400, #23427, #13414, #17853 ) ) ;
#13721 = DIRECTION ( 'NONE',  ( -4.183096374613631247E-18, 1.000000000000000000, 0.000000000000000000 ) ) ;
#13722 = FILL_AREA_STYLE_COLOUR ( '', #22355 ) ;
#13723 = COLOUR_RGB ( '',0.8941176470588234615, 0.8941176470588234615, 0.8941176470588234615 ) ;
#13725 = ORIENTED_EDGE ( 'NONE', *, *, #13422, .T. ) ;
#13724 = ORIENTED_EDGE ( 'NONE', *, *, #1046, .F. ) ;
#13726 = AXIS2_PLACEMENT_3D ( 'NONE', #19379, #3088, #16135 ) ;
#13727 = CARTESIAN_POINT ( 'NONE',  ( -163.0000000000000853, -494.4690652294805204, 30.00000000000653699 ) ) ;
#13728 = DIRECTION ( 'NONE',  ( 1.000000000000000000, 3.469446951953617640E-16, 8.673617379884035472E-17 ) ) ;
#13729 = CARTESIAN_POINT ( 'NONE',  ( 0.000000000000000000, -145.0000000000000284, -90.00000000000000000 ) ) ;
#13730 = ADVANCED_FACE ( 'NONE', ( #3027 ), #2903, .F. ) ;
#13731 = DIRECTION ( 'NONE',  ( -0.000000000000000000, -0.000000000000000000, 1.000000000000000000 ) ) ;
#13732 = CARTESIAN_POINT ( 'NONE',  ( 7.500000000000000000, 4.330127018922190096, -10.00000000000000000 ) ) ;
#13733 = ORIENTED_EDGE ( 'NONE', *, *, #22640, .F. ) ;
#13734 = EDGE_CURVE ( 'NONE', #20344, #19833, #5347, .T. ) ;
#13735 = CARTESIAN_POINT ( 'NONE',  ( -52.99999999999997158, 1.617115494935892976E-29, -0.000000000000000000 ) ) ;
#13736 = VECTOR ( 'NONE', #367, 1000.000000000000000 ) ;
#13737 = DIRECTION ( 'NONE',  ( 0.000000000000000000, -1.000000000000000000, 0.000000000000000000 ) ) ;
#13738 = CARTESIAN_POINT ( 'NONE',  ( 21.00000000000000355, 0.000000000000000000, 0.000000000000000000 ) ) ;
#13739 = EDGE_LOOP ( 'NONE', ( #23188, #6836, #18875, #717 ) ) ;
#13740 = LINE ( 'NONE', #19240, #18672 ) ;
#13741 = VERTEX_POINT ( 'NONE', #17646 ) ;
#13742 = CARTESIAN_POINT ( 'NONE',  ( -285.2000000000014666, -127.0000000000000568, 146.4928932188134638 ) ) ;
#13743 = CARTESIAN_POINT ( 'NONE',  ( -67.34999999999998010, -112.6666666666667140, 3.000000000000001332 ) ) ;
#13744 = ORIENTED_EDGE ( 'NONE', *, *, #3507, .T. ) ;
#13745 = CARTESIAN_POINT ( 'NONE',  ( -24.99999999999999645, 9.326071307568738836E-16, -145.0000059999999849 ) ) ;
#13746 = ORIENTED_EDGE ( 'NONE', *, *, #22567, .F. ) ;
#13747 = DIRECTION ( 'NONE',  ( 3.469446951953614682E-16, -1.000000000000000000, 3.483493295888648978E-15 ) ) ;
#13748 = DIRECTION ( 'NONE',  ( 0.8090169943749552228, -0.5877852522924623679, 0.000000000000000000 ) ) ;
#13749 = FACE_OUTER_BOUND ( 'NONE', #5159, .T. ) ;
#13750 = AXIS2_PLACEMENT_3D ( 'NONE', #14963, #20725, #5779 ) ;
#13751 = FACE_OUTER_BOUND ( 'NONE', #15882, .T. ) ;
#13752 = DIRECTION ( 'NONE',  ( -1.000000000000000000, -0.000000000000000000, -0.000000000000000000 ) ) ;
#13753 = ORIENTED_EDGE ( 'NONE', *, *, #15282, .T. ) ;
#13754 = EDGE_CURVE ( 'NONE', #3595, #12831, #14525, .T. ) ;
#13755 = EDGE_CURVE ( 'NONE', #733, #12183, #6501, .T. ) ;
#13756 = CARTESIAN_POINT ( 'NONE',  ( 0.000000000000000000, 0.000000000000000000, 0.000000000000000000 ) ) ;
#13757 = CARTESIAN_POINT ( 'NONE',  ( -3.999999999998910649, -1.658469974638591804, -3.531532913075256186 ) ) ;
#13758 = ORIENTED_EDGE ( 'NONE', *, *, #14467, .F. ) ;
#13759 = CIRCLE ( 'NONE', #16423, 10.00000000000000000 ) ;
#13760 = ORIENTED_EDGE ( 'NONE', *, *, #9057, .T. ) ;
#13761 = VECTOR ( 'NONE', #5799, 1000.000000000000000 ) ;
#13762 = FACE_OUTER_BOUND ( 'NONE', #7457, .T. ) ;
#13763 = DIRECTION ( 'NONE',  ( 1.000000000000000000, -0.000000000000000000, 6.982962677686266711E-15 ) ) ;
#13764 = ADVANCED_FACE ( 'NONE', ( #18016 ), #10798, .F. ) ;
#13766 = DIRECTION ( 'NONE',  ( -2.775557561562891351E-17, 1.000000000000000000, 0.000000000000000000 ) ) ;
#13765 = PRODUCT_DEFINITION_SHAPE ( 'NONE', 'NONE',  #23877 ) ;
#13767 = EDGE_CURVE ( 'NONE', #11303, #2646, #10777, .T. ) ;
#13768 = AXIS2_PLACEMENT_3D ( 'NONE', #18532, #439, #1986 ) ;
#13769 = CARTESIAN_POINT ( 'NONE',  ( 235.0000000000000284, -560.0000000000000000, -60.00000000000000711 ) ) ;
#13770 = DIRECTION ( 'NONE',  ( -0.000000000000000000, -0.000000000000000000, 1.000000000000000000 ) ) ;
#13771 = EDGE_CURVE ( 'NONE', #15265, #2756, #19566, .T. ) ;
#13772 = CARTESIAN_POINT ( 'NONE',  ( -56.99999999999995737, 1.739161947383884814E-29, -0.000000000000000000 ) ) ;
#13773 = VERTEX_POINT ( 'NONE', #10442 ) ;
#13774 = DIRECTION ( 'NONE',  ( 0.000000000000000000, -1.177509268541832635E-16, 1.000000000000000000 ) ) ;
#13775 = AXIS2_PLACEMENT_3D ( 'NONE', #3959, #4340, #15115 ) ;
#13776 = CARTESIAN_POINT ( 'NONE',  ( 80.00000000000000000, -62.00000000000001421, 5.199999999999997513 ) ) ;
#13777 = ORIENTED_EDGE ( 'NONE', *, *, #20857, .F. ) ;
#13778 = CARTESIAN_POINT ( 'NONE',  ( 282.1427398886702917, 268.3758453455903918, -146.2440776823444537 ) ) ;
#13779 = CIRCLE ( 'NONE', #3308, 2.700000000000000622 ) ;
#13780 = CARTESIAN_POINT ( 'NONE',  ( 16.55500000000001393, 0.000000000000000000, 0.000000000000000000 ) ) ;
#13781 = LINE ( 'NONE', #15464, #7290 ) ;
#13782 = FACE_OUTER_BOUND ( 'NONE', #13354, .T. ) ;
#13783 = ORIENTED_EDGE ( 'NONE', *, *, #9457, .F. ) ;
#13784 = ORIENTED_EDGE ( 'NONE', *, *, #18460, .F. ) ;
#13785 = DIRECTION ( 'NONE',  ( 1.000000000000000000, 0.000000000000000000, 0.000000000000000000 ) ) ;
#13786 = DIRECTION ( 'NONE',  ( 1.000000000000000000, 3.495664435217746592E-15, -0.000000000000000000 ) ) ;
#13787 = EDGE_LOOP ( 'NONE', ( #21028, #11471 ) ) ;
#13788 = ADVANCED_FACE ( 'NONE', ( #19935 ), #8490, .F. ) ;
#13789 = VECTOR ( 'NONE', #17083, 1000.000000000000000 ) ;
#13790 = EDGE_CURVE ( 'NONE', #18606, #23584, #22317, .T. ) ;
#13791 = VERTEX_POINT ( 'NONE', #5099 ) ;
#13792 = DIRECTION ( 'NONE',  ( -7.709882115452476934E-17, -1.000000000000000000, 0.000000000000000000 ) ) ;
#13793 = CYLINDRICAL_SURFACE ( 'NONE', #8773, 7.500000000000000000 ) ;
#13794 = VERTEX_POINT ( 'NONE', #21643 ) ;
#13795 = EDGE_CURVE ( 'NONE', #11293, #13591, #15867, .T. ) ;
#13796 = CARTESIAN_POINT ( 'NONE',  ( 2.500000000000000000, 2.357898499370431722, -2.818925648462311528E-15 ) ) ;
#13797 = ORIENTED_EDGE ( 'NONE', *, *, #16362, .F. ) ;
#13798 = EDGE_CURVE ( 'NONE', #15856, #3142, #10392, .T. ) ;
#13799 = TOROIDAL_SURFACE ( 'NONE', #3337, 5.400000000000002132, 0.4000000000000000222 ) ;
#13800 = LINE ( 'NONE', #21252, #19865 ) ;
#13801 = EDGE_CURVE ( 'NONE', #9344, #21582, #10541, .T. ) ;
#13802 = FACE_OUTER_BOUND ( 'NONE', #21344, .T. ) ;
#13803 = ORIENTED_EDGE ( 'NONE', *, *, #3122, .F. ) ;
#13804 = ORIENTED_EDGE ( 'NONE', *, *, #20695, .F. ) ;
#13805 = VERTEX_POINT ( 'NONE', #11033 ) ;
#13806 = CARTESIAN_POINT ( 'NONE',  ( -280.0000000000000568, -127.0000000000000568, -147.2000000000013245 ) ) ;
#13807 = CARTESIAN_POINT ( 'NONE',  ( 2.807080416178989513, -3.225969019225150003, -3.502507215260505014 ) ) ;
#13808 = DIRECTION ( 'NONE',  ( 1.000000000000000000, -4.183096374613631247E-18, 0.000000000000000000 ) ) ;
#13809 = DIRECTION ( 'NONE',  ( 0.000000000000000000, -0.000000000000000000, 1.000000000000000000 ) ) ;
#13810 = EDGE_LOOP ( 'NONE', ( #2602, #2442, #5468, #9050 ) ) ;
#13811 = CARTESIAN_POINT ( 'NONE',  ( -1.013163106016700565, -8.075304045852661261, -7.231838333420565590 ) ) ;
#13812 = CIRCLE ( 'NONE', #272, 2.649999999999971934 ) ;
#13813 = ORIENTED_EDGE ( 'NONE', *, *, #6361, .F. ) ;
#13814 = AXIS2_PLACEMENT_3D ( 'NONE', #5067, #21942, #2984 ) ;
#13815 = ORIENTED_EDGE ( 'NONE', *, *, #14759, .F. ) ;
#13816 = DIRECTION ( 'NONE',  ( 0.000000000000000000, -1.287488025362403787E-15, -1.000000000000000000 ) ) ;
#13817 = EDGE_LOOP ( 'NONE', ( #2289, #20214, #17863, #22187 ) ) ;
#13818 = PLANE ( 'NONE',  #20215 ) ;
#13819 = CARTESIAN_POINT ( 'NONE',  ( 72.64999999999999147, -87.33333333333332860, 3.000000000000001332 ) ) ;
#13820 = EDGE_LOOP ( 'NONE', ( #18288, #5836, #7986, #15569 ) ) ;
#13821 = B_SPLINE_CURVE_WITH_KNOTS ( 'NONE', 3,
 ( #22130, #23600, #5373, #12793, #20097, #13010, #16609, #9118, #3542, #65 ),
 .UNSPECIFIED., .F., .F.,
 ( 4, 2, 2, 2, 4 ),
 ( 0.01051144076094934904, 0.01162027323572610918, 0.01272910571050286932, 0.01383793818527962946, 0.01494677066005638960 ),
 .UNSPECIFIED. ) ;
#13822 = EDGE_CURVE ( 'NONE', #12, #7786, #3264, .T. ) ;
#13823 = CARTESIAN_POINT ( 'NONE',  ( -280.1244266425809428, 269.9696999999999889, 145.2840560642350169 ) ) ;
#13824 = DIRECTION ( 'NONE',  ( 6.753181414994864868E-15, 0.000000000000000000, -1.000000000000000000 ) ) ;
#13825 = EDGE_CURVE ( 'NONE', #10912, #874, #12722, .T. ) ;
#13826 = AXIS2_PLACEMENT_3D ( 'NONE', #21462, #1997, #1876 ) ;
#13827 = ORIENTED_EDGE ( 'NONE', *, *, #17778, .F. ) ;
#13828 = UNCERTAINTY_MEASURE_WITH_UNIT (LENGTH_MEASURE( 1.000000000000000082E-05 ), #11673, 'distance_accuracy_value', 'NONE');
#13829 = EDGE_CURVE ( 'NONE', #13423, #1301, #5817, .T. ) ;
#13830 = CARTESIAN_POINT ( 'NONE',  ( 30.00000000000000000, 2.054999999999997939, -6.938893903907228378E-15 ) ) ;
#13831 = AXIS2_PLACEMENT_3D ( 'NONE', #18368, #18031, #21766 ) ;
#13832 = CARTESIAN_POINT ( 'NONE',  ( -8.050072859967423611, -976.2745910299377101, -145.0000000000001137 ) ) ;
#13833 = CIRCLE ( 'NONE', #3367, 2.500000000000002220 ) ;
#13834 = CARTESIAN_POINT ( 'NONE',  ( 0.000000000000000000, 2.755455298081544778E-15, -22.50000000000000000 ) ) ;
#13835 = AXIS2_PLACEMENT_3D ( 'NONE', #14955, #7582, #5516 ) ;
#13836 = LINE ( 'NONE', #4621, #6899 ) ;
#13837 = ORIENTED_EDGE ( 'NONE', *, *, #15248, .T. ) ;
#13838 = FACE_OUTER_BOUND ( 'NONE', #21495, .T. ) ;
#13840 = VERTEX_POINT ( 'NONE', #11389 ) ;
#13839 = ORIENTED_EDGE ( 'NONE', *, *, #17174, .T. ) ;
#13841 = DIRECTION ( 'NONE',  ( -1.000000000000000000, 1.408839003528726857E-14, 0.000000000000000000 ) ) ;
#13842 = CARTESIAN_POINT ( 'NONE',  ( 80.00000000000001421, -56.79999999999998295, 5.199999999999985967 ) ) ;
#13843 = DIRECTION ( 'NONE',  ( -0.000000000000000000, 1.000000000000000000, -0.000000000000000000 ) ) ;
#13844 = AXIS2_PLACEMENT_3D ( 'NONE', #21205, #21559, #8180 ) ;
#13845 = CARTESIAN_POINT ( 'NONE',  ( -282.2000000000008981, 30.00000000000101963, -105.0000000000000142 ) ) ;
#13846 = CARTESIAN_POINT ( 'NONE',  ( -20.00000000000000000, 2.449293598294706513E-15, -150.0000000000000000 ) ) ;
#13847 = CARTESIAN_POINT ( 'NONE',  ( -281.3610889986683219, 272.8646579186752774, -145.2488155364688396 ) ) ;
#13848 = CIRCLE ( 'NONE', #11941, 2.500000000000002220 ) ;
#13849 = AXIS2_PLACEMENT_3D ( 'NONE', #20485, #2246, #9515 ) ;
#13850 = VERTEX_POINT ( 'NONE', #20281 ) ;
#13851 = AXIS2_PLACEMENT_3D ( 'NONE', #10111, #17455, #6229 ) ;
#13852 = FACE_OUTER_BOUND ( 'NONE', #2244, .T. ) ;
#13853 = CIRCLE ( 'NONE', #7632, 35.00000000000000711 ) ;
#13854 = DIRECTION ( 'NONE',  ( 1.000000000000000000, 0.000000000000000000, 0.000000000000000000 ) ) ;
#13855 = CARTESIAN_POINT ( 'NONE',  ( -146.4450000000000784, -784.4690652294805204, 30.00000000000641975 ) ) ;
#13856 = ORIENTED_EDGE ( 'NONE', *, *, #1516, .F. ) ;
#13857 = LINE ( 'NONE', #18884, #9445 ) ;
#13858 = ORIENTED_EDGE ( 'NONE', *, *, #11687, .F. ) ;
#13859 = DIRECTION ( 'NONE',  ( -1.110223024625157172E-14, 0.000000000000000000, -1.000000000000000000 ) ) ;
#13860 = CARTESIAN_POINT ( 'NONE',  ( 0.000000000000000000, 0.000000000000000000, 20.00000000000000000 ) ) ;
#13861 = ORIENTED_EDGE ( 'NONE', *, *, #12453, .F. ) ;
#13862 = CARTESIAN_POINT ( 'NONE',  ( -1.642023387316847050, 24.99995073929417444, -145.0000000000000000 ) ) ;
#13863 = ORIENTED_EDGE ( 'NONE', *, *, #9381, .T. ) ;
#13864 =( LENGTH_UNIT ( ) NAMED_UNIT ( * ) SI_UNIT ( .MILLI., .METRE. ) );
#13865 = DIRECTION ( 'NONE',  ( -1.000000000000000000, 0.000000000000000000, 0.000000000000000000 ) ) ;
#13866 = PRODUCT ( 'hex flange nut gradea_iso_ISO - 4161 - M5 - N', 'hex flange nut gradea_iso_ISO - 4161 - M5 - N', '', ( #226 ) ) ;
#13867 = CIRCLE ( 'NONE', #12345, 0.2000000000000000944 ) ;
#13868 = DIRECTION ( 'NONE',  ( 1.000000000000000000, 0.000000000000000000, 0.000000000000000000 ) ) ;
#13869 = AXIS2_PLACEMENT_3D ( 'NONE', #11758, #9921, #8792 ) ;
#13870 = LINE ( 'NONE', #21313, #17318 ) ;
#13871 = CARTESIAN_POINT ( 'NONE',  ( -3.861362476283256129, -2.629030857716004199, -3.671615880910374941 ) ) ;
#13872 = CONICAL_SURFACE ( 'NONE', #10776, 2.055000000000001492, 0.7853981633974633780 ) ;
#13873 = CARTESIAN_POINT ( 'NONE',  ( -52.99999999999996447, -56.79999999999978400, 73.75676759431465257 ) ) ;
#13874 = AXIS2_PLACEMENT_3D ( 'NONE', #8603, #7026, #14307 ) ;
#13875 = ORIENTED_EDGE ( 'NONE', *, *, #1676, .T. ) ;
#13876 = LINE ( 'NONE', #1266, #11130 ) ;
#13877 = CARTESIAN_POINT ( 'NONE',  ( 0.000000000000000000, 0.000000000000000000, -90.00000000000000000 ) ) ;
#13878 = ORIENTED_EDGE ( 'NONE', *, *, #7837, .F. ) ;
#13879 = ORIENTED_EDGE ( 'NONE', *, *, #17663, .F. ) ;
#13880 = CARTESIAN_POINT ( 'NONE',  ( -56.99999999999995737, -56.80000000000005400, 2.101443903218560127E-13 ) ) ;
#13881 = DIRECTION ( 'NONE',  ( 0.000000000000000000, 5.551115123125777969E-15, -1.000000000000000000 ) ) ;
#13882 = DIRECTION ( 'NONE',  ( 0.000000000000000000, 1.000000000000000000, -1.295896757998781966E-15 ) ) ;
#13883 = CIRCLE ( 'NONE', #16551, 4.250000000000000000 ) ;
#13884 = TOROIDAL_SURFACE ( 'NONE', #18146, 4.000000000000000000, 0.2500000000000000000 ) ;
#13885 = CARTESIAN_POINT ( 'NONE',  ( 132.0389103176321441, 81.18340533128269954, 28.00959664470845567 ) ) ;
#13886 = CARTESIAN_POINT ( 'NONE',  ( 45.00000000000000000, 272.9999999999999432, 5.249999999999973355 ) ) ;
#13887 = CIRCLE ( 'NONE', #22315, 145.0000000000000284 ) ;
#13888=STYLED_ITEM('',(#23927),#4039);
#13889 = AXIS2_PLACEMENT_3D ( 'NONE', #217, #9161, #20723 ) ;
#13890 = DIRECTION ( 'NONE',  ( 0.000000000000000000, 0.5000000000000009992, 0.8660254037844380415 ) ) ;
#13891 = ORIENTED_EDGE ( 'NONE', *, *, #11226, .F. ) ;
#13892 = ADVANCED_FACE ( 'NONE', ( #3511 ), #3738, .F. ) ;
#13893 = DIRECTION ( 'NONE',  ( -0.000000000000000000, -0.000000000000000000, -1.000000000000000000 ) ) ;
#13894 = CARTESIAN_POINT ( 'NONE',  ( 2.500000000000000000, -1.768423874527823569, 1.021000000000002794 ) ) ;
#13895 =( REPRESENTATION_RELATIONSHIP ('NONE','NONE', #10127, #22995 ) REPRESENTATION_RELATIONSHIP_WITH_TRANSFORMATION ( #10078 )SHAPE_REPRESENTATION_RELATIONSHIP( ) );
#13896 = EDGE_CURVE ( 'NONE', #3985, #19527, #16793, .T. ) ;
#13897 = CIRCLE ( 'NONE', #15404, 2.500000000000002220 ) ;
#13898 = ADVANCED_FACE ( 'NONE', ( #9330, #13222 ), #16564, .T. ) ;
#13899 = VERTEX_POINT ( 'NONE', #20524 ) ;
#13900 = CARTESIAN_POINT ( 'NONE',  ( -1.500000000000000000, 0.000000000000000000, -50.00000000000000000 ) ) ;
#13901 =( REPRESENTATION_RELATIONSHIP ('NONE','NONE', #10127, #18083 ) REPRESENTATION_RELATIONSHIP_WITH_TRANSFORMATION ( #6088 )SHAPE_REPRESENTATION_RELATIONSHIP( ) );
#13902 = APPLICATION_PROTOCOL_DEFINITION ( 'draft international standard', 'automotive_design', 1998, #12972 ) ;
#13903 = CARTESIAN_POINT ( 'NONE',  ( 2.500000000000000000, 2.357898499370431722, -2.818925648462311528E-15 ) ) ;
#13904 = CARTESIAN_POINT ( 'NONE',  ( -12.52393590864752682, -1021.698958664561019, -145.0000000000001421 ) ) ;
#13905 = ADVANCED_FACE ( 'NONE', ( #10918 ), #2046, .T. ) ;
#13906 = DIRECTION ( 'NONE',  ( -6.640089860198304064E-16, -1.000000000000000000, 0.000000000000000000 ) ) ;
#13907 = DIRECTION ( 'NONE',  ( -1.000000000000000000, 0.000000000000000000, 0.000000000000000000 ) ) ;
#13908 = VERTEX_POINT ( 'NONE', #9204 ) ;
#13909 = ORIENTED_EDGE ( 'NONE', *, *, #19227, .T. ) ;
#13910 = AXIS2_PLACEMENT_3D ( 'NONE', #16186, #23546, #7002 ) ;
#13911 = CARTESIAN_POINT ( 'NONE',  ( -280.8086578304520913, 269.2538215477169388, -146.6574776399288282 ) ) ;
#13912 = VECTOR ( 'NONE', #10617, 1000.000000000000000 ) ;
#13913 = DIRECTION ( 'NONE',  ( 0.000000000000000000, 0.000000000000000000, -1.000000000000000000 ) ) ;
#13914 = CIRCLE ( 'NONE', #23112, 2.649999999999985700 ) ;
#13915 = VECTOR ( 'NONE', #1123, 1000.000000000000000 ) ;
#13916 = ORIENTED_EDGE ( 'NONE', *, *, #18706, .F. ) ;
#13917 = AXIS2_PLACEMENT_3D ( 'NONE', #10100, #11561, #2578 ) ;
#13918 = AXIS2_PLACEMENT_3D ( 'NONE', #19748, #7069, #6835 ) ;
#13919 = ORIENTED_EDGE ( 'NONE', *, *, #12769, .F. ) ;
#13920 = DIRECTION ( 'NONE',  ( 1.000000000000000000, 0.000000000000000000, 0.000000000000000000 ) ) ;
#13921 = DIRECTION ( 'NONE',  ( 1.000000000000000000, 0.000000000000000000, 0.000000000000000000 ) ) ;
#13922 = ORIENTED_EDGE ( 'NONE', *, *, #16411, .F. ) ;
#13923 = CARTESIAN_POINT ( 'NONE',  ( 45.24999999999994316, 100.0000000000000000, 150.2000000000009550 ) ) ;
#13924 = ORIENTED_EDGE ( 'NONE', *, *, #23003, .F. ) ;
#13926 = VECTOR ( 'NONE', #23411, 1000.000000000000000 ) ;
#13925 = AXIS2_PLACEMENT_3D ( 'NONE', #534, #15277, #1467 ) ;
#13927 = DIRECTION ( 'NONE',  ( 3.469446951953614682E-16, -1.000000000000000000, 3.483493295888648978E-15 ) ) ;
#13929 = AXIS2_PLACEMENT_3D ( 'NONE', #3219, #15931, #10386 ) ;
#13928 = CARTESIAN_POINT ( 'NONE',  ( -3.000000000000001332, 23.97500000000000142, 0.000000000000000000 ) ) ;
#13930 = ORIENTED_EDGE ( 'NONE', *, *, #14119, .T. ) ;
#13931 = VERTEX_POINT ( 'NONE', #18590 ) ;
#13932 = DIRECTION ( 'NONE',  ( -3.700743415417188731E-15, -1.000000000000000000, -0.000000000000000000 ) ) ;
#13933 = CONICAL_SURFACE ( 'NONE', #8886, 2.055000000000001492, 0.7853981633974633780 ) ;
#13934 = AXIS2_PLACEMENT_3D ( 'NONE', #8055, #9871, #11339 ) ;
#13935 = CARTESIAN_POINT ( 'NONE',  ( -0.1750025118121544265, -4.719839900820635314, -3.469254087858253399 ) ) ;
#13936 = EDGE_CURVE ( 'NONE', #15352, #9513, #387, .T. ) ;
#13937 = DIRECTION ( 'NONE',  ( 1.000000000000000000, -0.000000000000000000, 6.982962677686266711E-15 ) ) ;
#13938 = DIRECTION ( 'NONE',  ( -0.000000000000000000, 0.000000000000000000, -1.000000000000000000 ) ) ;
#13939 = VECTOR ( 'NONE', #3163, 1000.000000000000114 ) ;
#13940 = EDGE_CURVE ( 'NONE', #20633, #21635, #22698, .T. ) ;
#13941 = ORIENTED_EDGE ( 'NONE', *, *, #17653, .F. ) ;
#13942 = CARTESIAN_POINT ( 'NONE',  ( 2.500000000000002220, 1.178949249685212086, -2.042000000000002036 ) ) ;
#13943 = EDGE_CURVE ( 'NONE', #12485, #19969, #9081, .T. ) ;
#13944 = ORIENTED_EDGE ( 'NONE', *, *, #10043, .F. ) ;
#13945 = AXIS2_PLACEMENT_3D ( 'NONE', #18386, #4825, #21485 ) ;
#13946 = EDGE_CURVE ( 'NONE', #11930, #18385, #23791, .T. ) ;
#13947 = AXIS2_PLACEMENT_3D ( 'NONE', #13402, #5874, #20965 ) ;
#13948 = CIRCLE ( 'NONE', #4650, 2.649999999999992806 ) ;
#13949 = AXIS2_PLACEMENT_3D ( 'NONE', #4386, #20926, #9960 ) ;
#13950 = ORIENTED_EDGE ( 'NONE', *, *, #12779, .T. ) ;
#13951 = CARTESIAN_POINT ( 'NONE',  ( -3.267023609986814847, -24.83987733669349751, -145.0000000000000000 ) ) ;
#13952 = ORIENTED_EDGE ( 'NONE', *, *, #19297, .F. ) ;
#13953 = DIRECTION ( 'NONE',  ( 0.8191520442889907994, 0.000000000000000000, 0.5735764363510474917 ) ) ;
#13954 = DIRECTION ( 'NONE',  ( 0.000000000000000000, 0.000000000000000000, 1.000000000000000000 ) ) ;
#13955 = ORIENTED_EDGE ( 'NONE', *, *, #19153, .F. ) ;
#13956 = FACE_OUTER_BOUND ( 'NONE', #19940, .T. ) ;
#13957 = DIRECTION ( 'NONE',  ( 0.000000000000000000, 0.000000000000000000, -1.000000000000000000 ) ) ;
#13958 = VERTEX_POINT ( 'NONE', #1938 ) ;
#13959 = FACE_OUTER_BOUND ( 'NONE', #14292, .T. ) ;
#13960 = CARTESIAN_POINT ( 'NONE',  ( 0.000000000000000000, 0.000000000000000000, -8.499999999999998224 ) ) ;
#13961 = CARTESIAN_POINT ( 'NONE',  ( -1.305263714129178521, 8.377797850839286298, -7.792447862505335721 ) ) ;
#13962 = CARTESIAN_POINT ( 'NONE',  ( 0.000000000000000000, 0.000000000000000000, -90.00000000000000000 ) ) ;
#13963 = ORIENTED_EDGE ( 'NONE', *, *, #2358, .F. ) ;
#13964 = CARTESIAN_POINT ( 'NONE',  ( -2.699999999999995737, 0.000000000000000000, 0.000000000000000000 ) ) ;
#13965 = PRODUCT_DEFINITION_SHAPE ( 'NONE', 'NONE',  #23879 ) ;
#13967 = ORIENTED_EDGE ( 'NONE', *, *, #1635, .F. ) ;
#13966 = VERTEX_POINT ( 'NONE', #14647 ) ;
#13968 = DIRECTION ( 'NONE',  ( 2.832769448823989808E-16, -1.000000000000000000, 3.469446951953613794E-15 ) ) ;
#13969 = EDGE_CURVE ( 'NONE', #17494, #1219, #12974, .T. ) ;
#13970 = ADVANCED_FACE ( 'NONE', ( #12862 ), #20167, .T. ) ;
#13971 = DIRECTION ( 'NONE',  ( -0.000000000000000000, 1.000000000000000000, -3.469446951953613794E-15 ) ) ;
#13972 = ADVANCED_FACE ( 'NONE', ( #15359 ), #13587, .F. ) ;
#13973 = CARTESIAN_POINT ( 'NONE',  ( 160.0000000000000000, 1.959434878635765210E-14, 90.00000000000000000 ) ) ;
#13974 = FACE_OUTER_BOUND ( 'NONE', #3544, .T. ) ;
#13975 = CARTESIAN_POINT ( 'NONE',  ( -282.1697000000000912, 267.7999999999999545, -146.4928932188134354 ) ) ;
#13976 = ORIENTED_EDGE ( 'NONE', *, *, #5514, .T. ) ;
#13977 = CARTESIAN_POINT ( 'NONE',  ( 2.122234012456543311E-14, -56.79999999999985505, 1.970645868709647558E-13 ) ) ;
#13978 = PLANE ( 'NONE',  #2091 ) ;
#13979 = CYLINDRICAL_SURFACE ( 'NONE', #18118, 20.00000000000000000 ) ;
#13980 = ORIENTED_EDGE ( 'NONE', *, *, #16662, .T. ) ;
#13981 = CARTESIAN_POINT ( 'NONE',  ( -0.6810597143197697489, -4.461075778259609770, -3.598441714920717516 ) ) ;
#13982 = EDGE_LOOP ( 'NONE', ( #18636, #12278, #17070, #6513 ) ) ;
#13983 = CARTESIAN_POINT ( 'NONE',  ( -160.0000000000000000, 0.000000000000000000, 100.0000000000000000 ) ) ;
#13984 = CARTESIAN_POINT ( 'NONE',  ( 119.6158142514527327, -1087.367367941136308, 30.00000000000641620 ) ) ;
#13985 = EDGE_LOOP ( 'NONE', ( #5778, #2638 ) ) ;
#13986 = CARTESIAN_POINT ( 'NONE',  ( 24.99999999999999645, -5.982013681773172432E-16, -145.0000059999999849 ) ) ;
#13987 = CARTESIAN_POINT ( 'NONE',  ( -7.499999999999999112, 41.99999999999998579, -100.0000000000000000 ) ) ;
#13988 = DIRECTION ( 'NONE',  ( -0.000000000000000000, 1.000000000000000000, 1.224646799147353207E-16 ) ) ;
#13989 = CARTESIAN_POINT ( 'NONE',  ( 2.500000000000002220, 0.000000000000000000, 0.000000000000000000 ) ) ;
#13990 = CARTESIAN_POINT ( 'NONE',  ( 280.2906609804447839, 269.9854425596107603, 145.1255802622536919 ) ) ;
#13991 = DIRECTION ( 'NONE',  ( -1.000000000000000000, 1.408839003528726857E-14, 6.982962677686266711E-15 ) ) ;
#13992 = DIRECTION ( 'NONE',  ( 0.5877852522924719159, 0.8090169943749482284, 0.000000000000000000 ) ) ;
#13993 = ORIENTED_EDGE ( 'NONE', *, *, #14182, .F. ) ;
#13994 = FACE_OUTER_BOUND ( 'NONE', #5239, .T. ) ;
#13995 = FACE_OUTER_BOUND ( 'NONE', #4747, .T. ) ;
#13996 = ORIENTED_EDGE ( 'NONE', *, *, #6325, .F. ) ;
#13997 = ORIENTED_EDGE ( 'NONE', *, *, #5892, .F. ) ;
#13998 = PLANE ( 'NONE',  #5365 ) ;
#13999 = DIRECTION ( 'NONE',  ( -0.000000000000000000, -0.000000000000000000, 1.000000000000000000 ) ) ;
#14000 = FACE_OUTER_BOUND ( 'NONE', #23195, .T. ) ;
#14001 = CARTESIAN_POINT ( 'NONE',  ( 132.7558223547125067, 80.00574117445309241, 32.50000000000647304 ) ) ;
#14002 = CARTESIAN_POINT ( 'NONE',  ( 3.000000000000002665, 2.877919977996280320E-15, 23.50000000000000000 ) ) ;
#14003 = DIRECTION ( 'NONE',  ( 0.000000000000000000, 0.8660254037844380415, -0.5000000000000009992 ) ) ;
#14004 = VERTEX_POINT ( 'NONE', #21016 ) ;
#14005 = CARTESIAN_POINT ( 'NONE',  ( -194.7500000000000284, -204.4690652294800657, 30.00000000000675726 ) ) ;
#14006 = DIRECTION ( 'NONE',  ( 0.000000000000000000, 0.000000000000000000, -1.000000000000000000 ) ) ;
#14007 = FILL_AREA_STYLE_COLOUR ( '', #19428 ) ;
#14008 = ORIENTED_EDGE ( 'NONE', *, *, #20616, .T. ) ;
#14009 = CARTESIAN_POINT ( 'NONE',  ( -0.2727178028658734932, 0.000000000000000000, 23.97500000000000497 ) ) ;
#14010 = DIRECTION ( 'NONE',  ( 1.000000000000000000, 0.000000000000000000, 0.000000000000000000 ) ) ;
#14011 = CARTESIAN_POINT ( 'NONE',  ( 11.08409875735507377, -1022.468567656124719, -145.0000000000001421 ) ) ;
#14012 = DIRECTION ( 'NONE',  ( 0.000000000000000000, 0.000000000000000000, -1.000000000000000000 ) ) ;
#14013 = PLANE ( 'NONE',  #16935 ) ;
#14014 = ADVANCED_FACE ( 'NONE', ( #15242 ), #21132, .F. ) ;
#14015 = DIRECTION ( 'NONE',  ( 0.000000000000000000, 0.000000000000000000, 1.000000000000000000 ) ) ;
#14016 = CIRCLE ( 'NONE', #8203, 19.99999999999998934 ) ;
#14017 = ORIENTED_EDGE ( 'NONE', *, *, #5514, .F. ) ;
#14018 = ORIENTED_EDGE ( 'NONE', *, *, #14740, .F. ) ;
#14019 = CARTESIAN_POINT ( 'NONE',  ( -280.6212670861564789, 269.5502846751312518, -146.3405375976306573 ) ) ;
#14020 = LINE ( 'NONE', #16046, #2292 ) ;
#14021 = ORIENTED_EDGE ( 'NONE', *, *, #16300, .T. ) ;
#14022 = ADVANCED_FACE ( 'NONE', ( #20897 ), #2659, .T. ) ;
#14023 = CARTESIAN_POINT ( 'NONE',  ( 155.0000000000000284, -499.9999999999999432, -59.99999999999997868 ) ) ;
#14024 = ADVANCED_FACE ( 'NONE', ( #4476 ), #2415, .T. ) ;
#14025 = EDGE_LOOP ( 'NONE', ( #11445, #8385, #20754, #7670 ) ) ;
#14026 = CARTESIAN_POINT ( 'NONE',  ( 280.2488155364687827, 272.8938770989752811, 146.3689414351990763 ) ) ;
#14027 = CARTESIAN_POINT ( 'NONE',  ( -126.5312127422334498, 89.52572971382257094, 30.80845853161017800 ) ) ;
#14028 = EDGE_LOOP ( 'NONE', ( #2799, #10598, #16939, #2527, #15853 ) ) ;
#14029 = CARTESIAN_POINT ( 'NONE',  ( -287.4000000000014552, -129.2000000000000455, 146.4928932188134638 ) ) ;
#14030 = EDGE_CURVE ( 'NONE', #3613, #8918, #6286, .T. ) ;
#14031 = AXIS2_PLACEMENT_3D ( 'NONE', #3000, #12491, #2878 ) ;
#14032 = ORIENTED_EDGE ( 'NONE', *, *, #10132, .T. ) ;
#14033 = DIRECTION ( 'NONE',  ( 0.000000000000000000, -1.000000000000000000, 1.471414886128461471E-15 ) ) ;
#14034 = LINE ( 'NONE', #2991, #3986 ) ;
#14035 = ORIENTED_EDGE ( 'NONE', *, *, #2472, .F. ) ;
#14036 = ORIENTED_EDGE ( 'NONE', *, *, #6456, .F. ) ;
#14037 = CARTESIAN_POINT ( 'NONE',  ( 133.4124711242730541, 78.90586732742340814, -32.24959887471651854 ) ) ;
#14038 = CARTESIAN_POINT ( 'NONE',  ( -277.2000000000009550, 35.00000000000096634, 105.0000000000000000 ) ) ;
#14039 = CARTESIAN_POINT ( 'NONE',  ( 1.257172072275274388, -3.892973519170983110, -3.433252694550781303 ) ) ;
#14040 = CARTESIAN_POINT ( 'NONE',  ( -288.2000000000006708, 90.00000000000100897, 37.64999999999996305 ) ) ;
#14041 = DIRECTION ( 'NONE',  ( 1.000000000000000000, 0.000000000000000000, 0.000000000000000000 ) ) ;
#14042 = ORIENTED_EDGE ( 'NONE', *, *, #15251, .F. ) ;
#14043 = DIRECTION ( 'NONE',  ( -0.000000000000000000, 1.000000000000000000, -3.469446951953613794E-15 ) ) ;
#14044 = SHAPE_REPRESENTATION_RELATIONSHIP ( 'NONE' , 'NONE' ,  #19462, #5011 ) ;
#14045 = CIRCLE ( 'NONE', #22091, 35.00000000000000000 ) ;
#14046 = VERTEX_POINT ( 'NONE', #6172 ) ;
#14047 = ADVANCED_FACE ( 'NONE', ( #19070 ), #4351, .F. ) ;
#14048 = ORIENTED_EDGE ( 'NONE', *, *, #13016, .T. ) ;
#14049 = CYLINDRICAL_SURFACE ( 'NONE', #15315, 5.249999999999942268 ) ;
#14050 = EDGE_LOOP ( 'NONE', ( #16097, #21714, #3344, #19685 ) ) ;
#14051 = CARTESIAN_POINT ( 'NONE',  ( 7.847095227763521308, 4.129731495738485414, -7.493596212620238894 ) ) ;
#14052 = EDGE_CURVE ( 'NONE', #18725, #6133, #20768, .T. ) ;
#14053 = CARTESIAN_POINT ( 'NONE',  ( -7.499999999999997335, 34.18698582794336005, -100.0000000000000000 ) ) ;
#14054 = CIRCLE ( 'NONE', #914, 2.041999999999999815 ) ;
#14055 = EDGE_CURVE ( 'NONE', #22842, #20948, #2269, .T. ) ;
#14056 = VERTEX_POINT ( 'NONE', #9924 ) ;
#14057 = CARTESIAN_POINT ( 'NONE',  ( 72.64999999999999147, -112.6666666666666714, 3.000000000000000000 ) ) ;
#14058 = CARTESIAN_POINT ( 'NONE',  ( -285.2000000000010687, -19.99999999999898392, 105.0000000000000000 ) ) ;
#14059 = ORIENTED_EDGE ( 'NONE', *, *, #423, .F. ) ;
#14060 = EDGE_CURVE ( 'NONE', #6254, #17523, #22337, .T. ) ;
#14061 = FACE_OUTER_BOUND ( 'NONE', #7727, .T. ) ;
#14062 = CARTESIAN_POINT ( 'NONE',  ( 7.808623696107882317, -4.508310992946666040, -7.999704684617485739 ) ) ;
#14063 = EDGE_CURVE ( 'NONE', #21765, #15297, #22576, .T. ) ;
#14064 = LINE ( 'NONE', #13640, #21192 ) ;
#14065 = CARTESIAN_POINT ( 'NONE',  ( -7.500000000000000000, -3.988190556646204588, -0.8526458641284329065 ) ) ;
#14066 = EDGE_LOOP ( 'NONE', ( #5444, #18000, #17877, #1197 ) ) ;
#14067 = DIRECTION ( 'NONE',  ( 1.000000000000000000, 0.000000000000000000, 0.000000000000000000 ) ) ;
#14068 =( REPRESENTATION_RELATIONSHIP ('NONE','NONE', #10127, #4815 ) REPRESENTATION_RELATIONSHIP_WITH_TRANSFORMATION ( #15685 )SHAPE_REPRESENTATION_RELATIONSHIP( ) );
#14069 = SURFACE_SIDE_STYLE ('',( #19339 ) ) ;
#14071 = ORIENTED_EDGE ( 'NONE', *, *, #2025, .T. ) ;
#14070 = VERTEX_POINT ( 'NONE', #11648 ) ;
#14072 = DIRECTION ( 'NONE',  ( 0.000000000000000000, 0.000000000000000000, 1.000000000000000000 ) ) ;
#14073 = CARTESIAN_POINT ( 'NONE',  ( 7.908217798048221781, 3.084840533507044125, -7.795645399445156443 ) ) ;
#14074 = DIRECTION ( 'NONE',  ( -0.000000000000000000, -0.000000000000000000, 1.000000000000000000 ) ) ;
#14075 = CARTESIAN_POINT ( 'NONE',  ( 5.200000000000002842, 0.000000000000000000, 0.000000000000000000 ) ) ;
#14076 = CARTESIAN_POINT ( 'NONE',  ( 287.4000000000013415, -127.0000000000000568, -146.4928932188134070 ) ) ;
#14077 = CARTESIAN_POINT ( 'NONE',  ( 2.500000000000000000, -1.178949249685213863, 2.042000000000002924 ) ) ;
#14078 = EDGE_CURVE ( 'NONE', #20948, #4643, #4097, .T. ) ;
#14079 = ORIENTED_EDGE ( 'NONE', *, *, #18138, .T. ) ;
#14080 = FACE_OUTER_BOUND ( 'NONE', #11099, .T. ) ;
#14081 = ORIENTED_EDGE ( 'NONE', *, *, #17286, .T. ) ;
#14082 = EDGE_CURVE ( 'NONE', #10936, #4595, #18826, .T. ) ;
#14083 = PLANE ( 'NONE',  #17912 ) ;
#14084 = VERTEX_POINT ( 'NONE', #7858 ) ;
#14085 = CARTESIAN_POINT ( 'NONE',  ( -282.2000000000008981, 30.00000000000101963, -102.3500000000000369 ) ) ;
#14086 = ORIENTED_EDGE ( 'NONE', *, *, #23180, .T. ) ;
#14087 = DIRECTION ( 'NONE',  ( -0.000000000000000000, -1.000000000000000000, -0.000000000000000000 ) ) ;
#14088 = CIRCLE ( 'NONE', #19430, 7.500000000000006217 ) ;
#14089 = CARTESIAN_POINT ( 'NONE',  ( 100.0000000000000000, -1400.000000000000000, -125.0000000000001705 ) ) ;
#14090 = EDGE_CURVE ( 'NONE', #21882, #12343, #6039, .T. ) ;
#14091 = ORIENTED_EDGE ( 'NONE', *, *, #21561, .T. ) ;
#14092 = EDGE_CURVE ( 'NONE', #17675, #3485, #1771, .T. ) ;
#14093 = DIRECTION ( 'NONE',  ( -1.000000000000000000, 1.408839003528726857E-14, 6.982962677686266711E-15 ) ) ;
#14094 = SURFACE_STYLE_FILL_AREA ( #19727 ) ;
#14095 = CYLINDRICAL_SURFACE ( 'NONE', #15751, 7.500000000000000000 ) ;
#14096 = CIRCLE ( 'NONE', #3625, 2.649999999999985700 ) ;
#14097 = CARTESIAN_POINT ( 'NONE',  ( 2.999999999999995559, 0.000000000000000000, 0.000000000000000000 ) ) ;
#14098 = DIRECTION ( 'NONE',  ( -0.6964005597823108573, 0.7176533009294141507, -6.982962677686267499E-15 ) ) ;
#14099 = CARTESIAN_POINT ( 'NONE',  ( 1.211595439868046853, -7.960739084487661543, -0.4504974108212073114 ) ) ;
#14100 = CARTESIAN_POINT ( 'NONE',  ( 5.000000000000000000, -3.755786496842898268E-15, -4.057500000000000107 ) ) ;
#14101 = ORIENTED_EDGE ( 'NONE', *, *, #22136, .T. ) ;
#14102 = CARTESIAN_POINT ( 'NONE',  ( 0.000000000000000000, -145.0000000000000284, -90.00000000000000000 ) ) ;
#14103 = DIRECTION ( 'NONE',  ( -0.7071067811865254793, 8.659560562355202797E-17, -0.7071067811865695552 ) ) ;
#14104 = EDGE_LOOP ( 'NONE', ( #18261, #23801, #8530, #16043, #2172, #15831, #16346, #15408 ) ) ;
#14105 = ORIENTED_EDGE ( 'NONE', *, *, #12291, .F. ) ;
#14106 = CIRCLE ( 'NONE', #3637, 2.649999999999989253 ) ;
#14107 = DIRECTION ( 'NONE',  ( 0.000000000000000000, -1.000000000000000000, 0.000000000000000000 ) ) ;
#14108 = DIRECTION ( 'NONE',  ( 0.000000000000000000, 0.000000000000000000, -1.000000000000000000 ) ) ;
#14109 = CARTESIAN_POINT ( 'NONE',  ( -288.2000000000011255, -29.99999999999898037, -102.3500000000000227 ) ) ;
#14110 = CONICAL_SURFACE ( 'NONE', #17533, 7.500000000000001776, 0.8594454914424796144 ) ;
#14111 = EDGE_CURVE ( 'NONE', #8474, #14788, #20487, .T. ) ;
#14112 = CARTESIAN_POINT ( 'NONE',  ( 132.0350058597967404, 81.18997658688670072, 32.00444854364500458 ) ) ;
#14113 = DIRECTION ( 'NONE',  ( 1.000000000000000000, 0.000000000000000000, 0.000000000000000000 ) ) ;
#14114 = ORIENTED_EDGE ( 'NONE', *, *, #183, .F. ) ;
#14115 = DIRECTION ( 'NONE',  ( -0.000000000000000000, 0.000000000000000000, 1.000000000000000000 ) ) ;
#14116 = ORIENTED_EDGE ( 'NONE', *, *, #17472, .F. ) ;
#14117 = DIRECTION ( 'NONE',  ( -1.000000000000000000, 0.000000000000000000, 0.000000000000000000 ) ) ;
#14118 = CARTESIAN_POINT ( 'NONE',  ( -4.000000000000000000, -2.309401076758512694, -3.433295621305382461 ) ) ;
#14119 = EDGE_CURVE ( 'NONE', #18305, #13199, #9243, .T. ) ;
#14120 = VECTOR ( 'NONE', #15322, 1000.000000000000000 ) ;
#14121 = VERTEX_POINT ( 'NONE', #20599 ) ;
#14122 = LINE ( 'NONE', #6973, #21909 ) ;
#14123 = FACE_OUTER_BOUND ( 'NONE', #21452, .T. ) ;
#14124 = EDGE_CURVE ( 'NONE', #1461, #326, #5527, .T. ) ;
#14125 = LINE ( 'NONE', #17718, #9281 ) ;
#14126 = CARTESIAN_POINT ( 'NONE',  ( 21.69895866468613121, -1012.523935908702356, -145.0000000000001421 ) ) ;
#14127 = PLANE ( 'NONE',  #12702 ) ;
#14128 = CARTESIAN_POINT ( 'NONE',  ( 5.000000000000000000, 4.685197434473814759, -5.637851296924623057E-15 ) ) ;
#14129 = CARTESIAN_POINT ( 'NONE',  ( -2.499999999999999556, 3.061616997868382648E-16, 3.469446951953614189E-15 ) ) ;
#14130 = AXIS2_PLACEMENT_3D ( 'NONE', #6751, #6392, #15834 ) ;
#14131 = CIRCLE ( 'NONE', #18655, 5.199999999999982414 ) ;
#14132 = ORIENTED_EDGE ( 'NONE', *, *, #4432, .T. ) ;
#14133 = ORIENTED_EDGE ( 'NONE', *, *, #1028, .F. ) ;
#14134 = CARTESIAN_POINT ( 'NONE',  ( 5.200000000000020606, 0.000000000000000000, -6.938893903907228378E-15 ) ) ;
#14135 = DIRECTION ( 'NONE',  ( -0.3090169943749370707, -0.9510565162951569729, 0.000000000000000000 ) ) ;
#14136 = ORIENTED_EDGE ( 'NONE', *, *, #18714, .F. ) ;
#14137 = DIRECTION ( 'NONE',  ( -2.775557561562891351E-17, 1.000000000000000000, 4.694093751100962712E-16 ) ) ;
#14138 = CARTESIAN_POINT ( 'NONE',  ( 0.6920835326022565237, 4.454600218803884459, -3.597382984111579862 ) ) ;
#14139 = CIRCLE ( 'NONE', #22190, 2.649999999999971934 ) ;
#14140 = ORIENTED_EDGE ( 'NONE', *, *, #17356, .T. ) ;
#14141 = CARTESIAN_POINT ( 'NONE',  ( 280.4976310729377360, 272.3699028110927429, 147.6339272673398284 ) ) ;
#14142 = DIRECTION ( 'NONE',  ( 1.000000000000000000, 0.000000000000000000, 0.000000000000000000 ) ) ;
#14143 = AXIS2_PLACEMENT_3D ( 'NONE', #7123, #12850, #5316 ) ;
#14144 = ORIENTED_EDGE ( 'NONE', *, *, #3960, .F. ) ;
#14145 = LINE ( 'NONE', #10150, #21019 ) ;
#14146 = AXIS2_PLACEMENT_3D ( 'NONE', #22724, #15264, #18852 ) ;
#14147 = ORIENTED_EDGE ( 'NONE', *, *, #15346, .F. ) ;
#14148 = CARTESIAN_POINT ( 'NONE',  ( 90.00000000000000000, -74.99999999999998579, 0.000000000000000000 ) ) ;
#14149 = CARTESIAN_POINT ( 'NONE',  ( 24.99999999999998579, 45.00100000000064426, 124.9999999999998579 ) ) ;
#14150 = VERTEX_POINT ( 'NONE', #2249 ) ;
#14151 = ORIENTED_EDGE ( 'NONE', *, *, #2376, .F. ) ;
#14152 = DIRECTION ( 'NONE',  ( -0.7232617928448825673, 0.6905739489807055653, 6.982962677686266711E-15 ) ) ;
#14153 = PRODUCT_DEFINITION_SHAPE ( 'NONE', 'NONE',  #23858 ) ;
#14154 = ADVANCED_FACE ( 'NONE', ( #7452 ), #3827, .F. ) ;
#14155 =( NAMED_UNIT ( * ) SI_UNIT ( $, .STERADIAN. ) SOLID_ANGLE_UNIT ( ) );
#14156 = CARTESIAN_POINT ( 'NONE',  ( 0.5469614295415388128, -4.303013824935362663, -3.535263753543555598 ) ) ;
#14157 = CIRCLE ( 'NONE', #6413, 5.000000000000001776 ) ;
#14158 = DIRECTION ( 'NONE',  ( 0.000000000000000000, 0.000000000000000000, 1.000000000000000000 ) ) ;
#14159 = PLANE ( 'NONE',  #20529 ) ;
#14160 = ORIENTED_EDGE ( 'NONE', *, *, #20668, .F. ) ;
#14161 = DIRECTION ( 'NONE',  ( 0.000000000000000000, 0.000000000000000000, 1.000000000000000000 ) ) ;
#14162 = ORIENTED_EDGE ( 'NONE', *, *, #8374, .F. ) ;
#14163 = ORIENTED_EDGE ( 'NONE', *, *, #19012, .T. ) ;
#14164 = DIRECTION ( 'NONE',  ( -0.000000000000000000, 0.000000000000000000, 1.000000000000000000 ) ) ;
#14165 = ORIENTED_EDGE ( 'NONE', *, *, #21893, .T. ) ;
#14166 = CIRCLE ( 'NONE', #3709, 5.199999999999982414 ) ;
#14167 = CARTESIAN_POINT ( 'NONE',  ( 3.295171437449806451, 7.213553046161976567, -7.590212325761626744 ) ) ;
#14168 = ORIENTED_EDGE ( 'NONE', *, *, #18957, .F. ) ;
#14169 = DIRECTION ( 'NONE',  ( 0.000000000000000000, -3.495664435217746987E-15, 1.000000000000000000 ) ) ;
#14170 = DIRECTION ( 'NONE',  ( -0.000000000000000000, -0.000000000000000000, 1.000000000000000000 ) ) ;
#14171 = ORIENTED_EDGE ( 'NONE', *, *, #14981, .T. ) ;
#14172 = EDGE_CURVE ( 'NONE', #2834, #19823, #8867, .T. ) ;
#14173 = CARTESIAN_POINT ( 'NONE',  ( -1.317756351988340180, 3.857995168970202116, -0.04852650426601388955 ) ) ;
#14174 = CARTESIAN_POINT ( 'NONE',  ( 2.699999999999995737, 0.000000000000000000, 0.000000000000000000 ) ) ;
#14175 = EDGE_CURVE ( 'NONE', #10443, #45, #15794, .T. ) ;
#14176 = AXIS2_PLACEMENT_3D ( 'NONE', #13102, #18708, #16685 ) ;
#14177 = CARTESIAN_POINT ( 'NONE',  ( 5.200000000000020606, 3.306546357697854226E-16, 2.699999999999993516 ) ) ;
#14178 = DIRECTION ( 'NONE',  ( 1.110223024625157172E-14, 0.000000000000000000, -1.000000000000000000 ) ) ;
#14179 = ORIENTED_EDGE ( 'NONE', *, *, #20842, .F. ) ;
#14180 = DIRECTION ( 'NONE',  ( 0.000000000000000000, 0.4999999999999990008, -0.8660254037844391517 ) ) ;
#14181 = AXIS2_PLACEMENT_3D ( 'NONE', #12474, #23535, #3120 ) ;
#14182 = EDGE_CURVE ( 'NONE', #16635, #19884, #22061, .T. ) ;
#14183 = EDGE_CURVE ( 'NONE', #550, #1996, #1584, .T. ) ;
#14185 = ORIENTED_EDGE ( 'NONE', *, *, #8157, .F. ) ;
#14184 = ORIENTED_EDGE ( 'NONE', *, *, #21870, .T. ) ;
#14186 = DIRECTION ( 'NONE',  ( 6.123233995736766036E-17, 0.000000000000000000, -1.000000000000000000 ) ) ;
#14187 = DIRECTION ( 'NONE',  ( 0.000000000000000000, -0.000000000000000000, 1.000000000000000000 ) ) ;
#14188 = LINE ( 'NONE', #20072, #11906 ) ;
#14189 = CARTESIAN_POINT ( 'NONE',  ( -40.00000000000000000, 100.0000000000000000, 150.2000000000009550 ) ) ;
#14190 = CARTESIAN_POINT ( 'NONE',  ( -280.5679143846944044, 269.9132285165672442, -145.2488155364688396 ) ) ;
#14191 = EDGE_CURVE ( 'NONE', #13282, #20887, #19253, .T. ) ;
#14192 = ORIENTED_EDGE ( 'NONE', *, *, #17042, .T. ) ;
#14193 = CIRCLE ( 'NONE', #5309, 20.00000000000001776 ) ;
#14194 =( REPRESENTATION_RELATIONSHIP ('NONE','NONE', #10127, #2341 ) REPRESENTATION_RELATIONSHIP_WITH_TRANSFORMATION ( #20871 )SHAPE_REPRESENTATION_RELATIONSHIP( ) );
#14195 = DIRECTION ( 'NONE',  ( 0.000000000000000000, 0.5000000000000009992, 0.8660254037844380415 ) ) ;
#14196 = EDGE_LOOP ( 'NONE', ( #8145, #9793, #16814, #7750 ) ) ;
#14197 = VECTOR ( 'NONE', #18501, 1000.000000000000000 ) ;
#14198 = DIRECTION ( 'NONE',  ( 1.000000000000000000, 0.000000000000000000, -0.000000000000000000 ) ) ;
#14199 = CIRCLE ( 'NONE', #16877, 2.055000000000001492 ) ;
#14200 = ORIENTED_EDGE ( 'NONE', *, *, #1639, .F. ) ;
#14201 = CARTESIAN_POINT ( 'NONE',  ( 285.1999999999999318, 267.7999999999999545, -146.4928932188133786 ) ) ;
#14202 = VERTEX_POINT ( 'NONE', #22295 ) ;
#14203 = CARTESIAN_POINT ( 'NONE',  ( -128.8385278530642495, 86.17219694792784423, -31.88744336596579387 ) ) ;
#14204 = CARTESIAN_POINT ( 'NONE',  ( -145.0000000000000284, -1000.000000000000000, -90.00000000000000000 ) ) ;
#14205 = VERTEX_POINT ( 'NONE', #1892 ) ;
#14206 = CARTESIAN_POINT ( 'NONE',  ( 3.678949249685231848, 5.299604027854762026E-17, 0.000000000000000000 ) ) ;
#14207 = CARTESIAN_POINT ( 'NONE',  ( 119.9257125005558891, -1087.686723660049893, 27.50000000000641975 ) ) ;
#14208 = CARTESIAN_POINT ( 'NONE',  ( 35.00000000000000711, -3.880967142342036772E-28, -147.2000000000008981 ) ) ;
#14209 = DIRECTION ( 'NONE',  ( -0.000000000000000000, -1.000000000000000000, -0.000000000000000000 ) ) ;
#14210 = CARTESIAN_POINT ( 'NONE',  ( -7.499999999999999112, 0.000000000000000000, -100.0000000000000000 ) ) ;
#14211 = CARTESIAN_POINT ( 'NONE',  ( -1.994931997373328159E-14, -8.660254037844390851, -1.000000000000000888 ) ) ;
#14212 = EDGE_CURVE ( 'NONE', #5557, #15698, #11113, .T. ) ;
#14213 = CIRCLE ( 'NONE', #23540, 5.199999999999982414 ) ;
#14214 = FACE_BOUND ( 'NONE', #5976, .T. ) ;
#14215 = EDGE_CURVE ( 'NONE', #21432, #10033, #22718, .T. ) ;
#14216 = ORIENTED_EDGE ( 'NONE', *, *, #2643, .F. ) ;
#14217 = ADVANCED_FACE ( 'NONE', ( #22533 ), #16648, .T. ) ;
#14218 = CARTESIAN_POINT ( 'NONE',  ( -110.0000000000000142, 95.00000000000001421, 0.000000000000000000 ) ) ;
#14219 = AXIS2_PLACEMENT_3D ( 'NONE', #7762, #13117, #9818 ) ;
#14220 = CARTESIAN_POINT ( 'NONE',  ( -4.000000000000000000, -2.472261339043343220, -3.687027428081192326 ) ) ;
#14221 = AXIS2_PLACEMENT_3D ( 'NONE', #1638, #3672, #5861 ) ;
#14222 = EDGE_LOOP ( 'NONE', ( #13577, #18084, #4470, #21630 ) ) ;
#14223 = VERTEX_POINT ( 'NONE', #2127 ) ;
#14224 = AXIS2_PLACEMENT_3D ( 'NONE', #1356, #16100, #5224 ) ;
#14225 = ADVANCED_FACE ( 'NONE', ( #18660 ), #19382, .T. ) ;
#14226 = DIRECTION ( 'NONE',  ( 0.000000000000000000, 0.000000000000000000, 1.000000000000000000 ) ) ;
#14227 = CARTESIAN_POINT ( 'NONE',  ( 0.000000000000000000, 1.865214261513747767E-15, -145.0000119999999697 ) ) ;
#14228 = EDGE_CURVE ( 'NONE', #16080, #19722, #23006, .T. ) ;
#14229 = EDGE_CURVE ( 'NONE', #14733, #218, #11605, .T. ) ;
#14230 = CARTESIAN_POINT ( 'NONE',  ( -282.1697000000000912, 268.0840560642351988, 146.3684665762324357 ) ) ;
#14231 = CARTESIAN_POINT ( 'NONE',  ( 279.9999999999999432, 269.9999999999999432, -144.9999999999999716 ) ) ;
#14232 = DIRECTION ( 'NONE',  ( 1.000000000000000000, 0.000000000000000000, -0.000000000000000000 ) ) ;
#14233 = VERTEX_POINT ( 'NONE', #2611 ) ;
#14234 = DIRECTION ( 'NONE',  ( 0.000000000000000000, 1.000000000000000000, 0.000000000000000000 ) ) ;
#14235 = EDGE_LOOP ( 'NONE', ( #4583, #22496, #22237, #11323 ) ) ;
#14236 = FACE_OUTER_BOUND ( 'NONE', #7892, .T. ) ;
#14237 = PLANE ( 'NONE',  #23076 ) ;
#14238 = AXIS2_PLACEMENT_3D ( 'NONE', #23515, #23259, #1044 ) ;
#14239 = AXIS2_PLACEMENT_3D ( 'NONE', #6123, #20720, #15449 ) ;
#14240 = LINE ( 'NONE', #3098, #9812 ) ;
#14241 = AXIS2_PLACEMENT_3D ( 'NONE', #3360, #17869, #23654 ) ;
#14242 = ORIENTED_EDGE ( 'NONE', *, *, #1472, .F. ) ;
#14243 = CARTESIAN_POINT ( 'NONE',  ( 70.00000000000000000, -87.33333333333332860, 124.9999999999999858 ) ) ;
#14244 = VECTOR ( 'NONE', #3932, 1000.000000000000000 ) ;
#14245 = CARTESIAN_POINT ( 'NONE',  ( 6.293430271071537518, -5.026740376715104652, -0.4524126574264552558 ) ) ;
#14246 = FACE_OUTER_BOUND ( 'NONE', #15418, .T. ) ;
#14247 = DIRECTION ( 'NONE',  ( -1.110223024625157172E-14, 0.000000000000000000, -1.000000000000000000 ) ) ;
#14248 = DIRECTION ( 'NONE',  ( -0.9396926207859138680, 0.000000000000000000, -0.3420201433256536139 ) ) ;
#14249 = CYLINDRICAL_SURFACE ( 'NONE', #23091, 2.500000000000002220 ) ;
#14250 = CARTESIAN_POINT ( 'NONE',  ( -281.6795879751485359, 272.7329465209280102, 145.3118087683467934 ) ) ;
#14251 = EDGE_LOOP ( 'NONE', ( #1388, #1369, #3216, #23629, #20861, #4756, #23589 ) ) ;
#14252 = VERTEX_POINT ( 'NONE', #7940 ) ;
#14253 = DIRECTION ( 'NONE',  ( -0.000000000000000000, -0.000000000000000000, 1.000000000000000000 ) ) ;
#14254 = CARTESIAN_POINT ( 'NONE',  ( 280.1255313583545785, 270.0000000000000568, 145.2905802150185650 ) ) ;
#14255 = ORIENTED_EDGE ( 'NONE', *, *, #7841, .T. ) ;
#14256 = PRODUCT_DEFINITION_SHAPE ( 'NONE', 'NONE',  #23811 ) ;
#14257 = CARTESIAN_POINT ( 'NONE',  ( 0.000000000000000000, 0.000000000000000000, 90.00000000000000000 ) ) ;
#14258 = CARTESIAN_POINT ( 'NONE',  ( -79.99999999999995737, -138.0000000000000284, 3.000000000000000000 ) ) ;
#14259 = ADVANCED_FACE ( 'NONE', ( #18919 ), #13523, .F. ) ;
#14260 = CIRCLE ( 'NONE', #6143, 2.649999999999985700 ) ;
#14261 = EDGE_CURVE ( 'NONE', #6335, #6867, #10009, .T. ) ;
#14262 = VECTOR ( 'NONE', #13622, 1000.000000000000000 ) ;
#14263 = CIRCLE ( 'NONE', #12739, 2.055000000000001492 ) ;
#14264 = EDGE_LOOP ( 'NONE', ( #21419, #12415, #5463, #13685 ) ) ;
#14265 = CARTESIAN_POINT ( 'NONE',  ( 281.3684637172357270, 268.4847249064869743, 150.2299999999999898 ) ) ;
#14266 = AXIS2_PLACEMENT_3D ( 'NONE', #16822, #13359, #20672 ) ;
#14267 = DIRECTION ( 'NONE',  ( -0.000000000000000000, -0.000000000000000000, -1.000000000000000000 ) ) ;
#14268 = ORIENTED_EDGE ( 'NONE', *, *, #14355, .F. ) ;
#14269 = CARTESIAN_POINT ( 'NONE',  ( -134.6777706902594787, -1076.726150876685324, -28.88328940716457893 ) ) ;
#14270 = AXIS2_PLACEMENT_3D ( 'NONE', #10455, #12053, #5109 ) ;
#14271 = EDGE_LOOP ( 'NONE', ( #6227, #10075, #4357, #7995 ) ) ;
#14272 = LINE ( 'NONE', #20330, #21022 ) ;
#14273 = DIRECTION ( 'NONE',  ( 0.000000000000000000, -0.5000000000000011102, -0.8660254037844379305 ) ) ;
#14274 = EDGE_LOOP ( 'NONE', ( #8604, #23359 ) ) ;
#14275 = ORIENTED_EDGE ( 'NONE', *, *, #21555, .T. ) ;
#14276 = CARTESIAN_POINT ( 'NONE',  ( -129.2206655591605511, -1072.408698320350595, 27.94500000000641649 ) ) ;
#14277 = CARTESIAN_POINT ( 'NONE',  ( 40.00000000000000000, 100.0000000000000000, 160.2000000000005855 ) ) ;
#14278 = PRESENTATION_LAYER_ASSIGNMENT (  '', '', ( #735 ) ) ;
#14279 = LINE ( 'NONE', #2771, #23157 ) ;
#14281 = VECTOR ( 'NONE', #21781, 1000.000000000000000 ) ;
#14280 =( GEOMETRIC_REPRESENTATION_CONTEXT ( 3 ) GLOBAL_UNCERTAINTY_ASSIGNED_CONTEXT ( ( #12845 ) ) GLOBAL_UNIT_ASSIGNED_CONTEXT ( ( #17994, #11454, #20477 ) ) REPRESENTATION_CONTEXT ( 'NONE', 'WORKASPACE' ) );
#14282 = VECTOR ( 'NONE', #8848, 1000.000000000000000 ) ;
#14284 = FACE_OUTER_BOUND ( 'NONE', #6972, .T. ) ;
#14283 = AXIS2_PLACEMENT_3D ( 'NONE', #13136, #1969, #3900 ) ;
#14285 = CIRCLE ( 'NONE', #17344, 5.560781378645573980 ) ;
#14286 = CARTESIAN_POINT ( 'NONE',  ( -288.2000000000011255, -29.99999999999898037, -105.0000000000000000 ) ) ;
#14287 = AXIS2_PLACEMENT_3D ( 'NONE', #13855, #21878, #3757 ) ;
#14288 = VECTOR ( 'NONE', #100, 1000.000000000000000 ) ;
#14289 = ORIENTED_EDGE ( 'NONE', *, *, #18033, .F. ) ;
#14290 = PLANE ( 'NONE',  #17248 ) ;
#14291 = EDGE_LOOP ( 'NONE', ( #9073, #12936, #17189, #14570 ) ) ;
#14292 = EDGE_LOOP ( 'NONE', ( #4329, #714, #23538, #4381 ) ) ;
#14293 = CARTESIAN_POINT ( 'NONE',  ( 194.7500000000002274, -210.0000000000003411, -32.49999999999322853 ) ) ;
#14295 = AXIS2_PLACEMENT_3D ( 'NONE', #6332, #16000, #8628 ) ;
#14294 = AXIS2_PLACEMENT_3D ( 'NONE', #18022, #1112, #4985 ) ;
#14296 = ORIENTED_EDGE ( 'NONE', *, *, #706, .F. ) ;
#14297 = CARTESIAN_POINT ( 'NONE',  ( -64.99999999999995737, -52.79999999999965610, 65.00000000000017053 ) ) ;
#14298 = VECTOR ( 'NONE', #1819, 1000.000000000000000 ) ;
#14299 = AXIS2_PLACEMENT_3D ( 'NONE', #16027, #18185, #14234 ) ;
#14300 = EDGE_LOOP ( 'NONE', ( #9018, #5826 ) ) ;
#14301 = CARTESIAN_POINT ( 'NONE',  ( -135.4018704341554269, -51.87806360044865528, -90.00000000000000000 ) ) ;
#14302 = EDGE_LOOP ( 'NONE', ( #2872, #19664, #5281, #19400, #20540 ) ) ;
#14303 = CARTESIAN_POINT ( 'NONE',  ( 21.00000000000000000, 2.055000000000000160, 0.000000000000000000 ) ) ;
#14304 = DIRECTION ( 'NONE',  ( 0.000000000000000000, -1.000000000000000000, -3.495664435217746987E-15 ) ) ;
#14305 = DIRECTION ( 'NONE',  ( 0.000000000000000000, 0.7071067811865462405, -0.7071067811865489050 ) ) ;
#14306 = DIRECTION ( 'NONE',  ( 0.000000000000000000, 0.000000000000000000, 1.000000000000000000 ) ) ;
#14307 = DIRECTION ( 'NONE',  ( 0.000000000000000000, -2.618450529776313049E-15, -1.000000000000000000 ) ) ;
#14308 = VERTEX_POINT ( 'NONE', #22891 ) ;
#14309 = AXIS2_PLACEMENT_3D ( 'NONE', #16187, #23548, #1207 ) ;
#14310 = CARTESIAN_POINT ( 'NONE',  ( 110.0000000000000000, -74.99999999999998579, 3.000000000000000000 ) ) ;
#14311 =( NAMED_UNIT ( * ) PLANE_ANGLE_UNIT ( ) SI_UNIT ( $, .RADIAN. ) );
#14312 = VECTOR ( 'NONE', #5030, 1000.000000000000000 ) ;
#14313 = EDGE_CURVE ( 'NONE', #8518, #18124, #11724, .T. ) ;
#14314 = AXIS2_PLACEMENT_3D ( 'NONE', #13903, #8425, #21231 ) ;
#14315 = AXIS2_PLACEMENT_3D ( 'NONE', #13279, #13532, #7807 ) ;
#14317 = ORIENTED_EDGE ( 'NONE', *, *, #23692, .F. ) ;
#14316 = VERTEX_POINT ( 'NONE', #15451 ) ;
#14318 = CARTESIAN_POINT ( 'NONE',  ( 0.000000000000000000, 0.000000000000000000, 200.0000000000000000 ) ) ;
#14319 = CARTESIAN_POINT ( 'NONE',  ( 0.2500000000000002220, 5.204748896376250699E-16, -4.250000000000000000 ) ) ;
#14320 = CARTESIAN_POINT ( 'NONE',  ( 281.4928932188134354, 267.8000000000000114, -150.2299999999999329 ) ) ;
#14321 = CYLINDRICAL_SURFACE ( 'NONE', #10795, 2.649999999999985700 ) ;
#14322 = EDGE_CURVE ( 'NONE', #11160, #326, #9763, .T. ) ;
#14323 = CARTESIAN_POINT ( 'NONE',  ( 281.4928932188134354, -127.0000000000000568, -152.4000000000012847 ) ) ;
#14324 = ORIENTED_EDGE ( 'NONE', *, *, #20932, .T. ) ;
#14325 = EDGE_CURVE ( 'NONE', #1314, #19715, #18844, .T. ) ;
#14326 = DIRECTION ( 'NONE',  ( 1.000000000000000000, 0.000000000000000000, 0.000000000000000000 ) ) ;
#14327 = ORIENTED_EDGE ( 'NONE', *, *, #15714, .T. ) ;
#14328 = DIRECTION ( 'NONE',  ( -0.000000000000000000, 1.000000000000000000, 1.224646799147353207E-16 ) ) ;
#14329 = CARTESIAN_POINT ( 'NONE',  ( -72.64999999999996305, -112.6666666666667140, 3.000000000000000000 ) ) ;
#14330 = CARTESIAN_POINT ( 'NONE',  ( 57.99999999999999289, -56.80000000000001137, 2.055021403285668792E-13 ) ) ;
#14331 = ADVANCED_FACE ( 'NONE', ( #2843 ), #11968, .F. ) ;
#14332 = EDGE_LOOP ( 'NONE', ( #11530, #22656, #22027, #22162 ) ) ;
#14333 = ORIENTED_EDGE ( 'NONE', *, *, #241, .F. ) ;
#14334 = CARTESIAN_POINT ( 'NONE',  ( -128.7674363984956756, 86.27842408395288487, -31.99040335529151946 ) ) ;
#14335 = ORIENTED_EDGE ( 'NONE', *, *, #11316, .F. ) ;
#14336 = CARTESIAN_POINT ( 'NONE',  ( -281.0571358042176939, 270.1059783239181797, 149.6730547946947354 ) ) ;
#14337 = CARTESIAN_POINT ( 'NONE',  ( 133.4862419878492688, 78.78097527456812088, 27.82653936295257324 ) ) ;
#14338 = DIRECTION ( 'NONE',  ( 1.000000000000000000, 0.000000000000000000, 0.000000000000000000 ) ) ;
#14339 = DIRECTION ( 'NONE',  ( 0.000000000000000000, 0.000000000000000000, 1.000000000000000000 ) ) ;
#14340 = FACE_OUTER_BOUND ( 'NONE', #15023, .T. ) ;
#14341 = CARTESIAN_POINT ( 'NONE',  ( 2.500000000000000000, 0.000000000000000000, 0.000000000000000000 ) ) ;
#14342 = FACE_BOUND ( 'NONE', #5500, .T. ) ;
#14343 = ORIENTED_EDGE ( 'NONE', *, *, #23070, .T. ) ;
#14344 = CARTESIAN_POINT ( 'NONE',  ( -7.500000000000000888, 2.886751345948126435, -7.198902722707427593 ) ) ;
#14345 = CARTESIAN_POINT ( 'NONE',  ( 0.02448733951239481094, 4.877042772274728044, -3.751161874094022242 ) ) ;
#14346 = APPLICATION_CONTEXT ( 'automotive_design' ) ;
#14347 = ORIENTED_EDGE ( 'NONE', *, *, #22341, .F. ) ;
#14348 = DIRECTION ( 'NONE',  ( -0.000000000000000000, -1.000000000000000000, 6.123233995736766036E-17 ) ) ;
#14349 = DIRECTION ( 'NONE',  ( -2.775557561562891351E-17, 1.000000000000000000, 4.694093751100962712E-16 ) ) ;
#14351 = CARTESIAN_POINT ( 'NONE',  ( -281.9223300543794721, 268.9079617568158938, 145.9952621458756425 ) ) ;
#14350 = PRODUCT_DEFINITION_SHAPE ( 'NONE', 'NONE',  #23821 ) ;
#14352 = EDGE_CURVE ( 'NONE', #19450, #1864, #15018, .T. ) ;
#14353 = LINE ( 'NONE', #14566, #18738 ) ;
#14354 = CARTESIAN_POINT ( 'NONE',  ( -285.1663417894422992, 268.4816199723480281, -146.3683070494394940 ) ) ;
#14355 = EDGE_CURVE ( 'NONE', #404, #14202, #361, .T. ) ;
#14356 = ORIENTED_EDGE ( 'NONE', *, *, #17286, .F. ) ;
#14357 = PLANE ( 'NONE',  #1121 ) ;
#14358 = EDGE_CURVE ( 'NONE', #20294, #22350, #6920, .T. ) ;
#14359 = EDGE_LOOP ( 'NONE', ( #21489, #2787, #21678, #1211 ) ) ;
#14360 = CARTESIAN_POINT ( 'NONE',  ( 2.500000000000000000, 1.178949249685218081, 2.041999999999998483 ) ) ;
#14361 = CARTESIAN_POINT ( 'NONE',  ( -281.4928932188134354, -132.2000000000000455, -177.2000000000013529 ) ) ;
#14362 = DIRECTION ( 'NONE',  ( -0.9423651898111409242, -0.3345860861306287903, 6.982962677686267499E-15 ) ) ;
#14363 = ORIENTED_EDGE ( 'NONE', *, *, #17444, .F. ) ;
#14364 = CARTESIAN_POINT ( 'NONE',  ( -44.80746418436748968, 137.9031948627972781, -90.00000000000000000 ) ) ;
#14365 = EDGE_CURVE ( 'NONE', #9157, #963, #8193, .T. ) ;
#14366 = CARTESIAN_POINT ( 'NONE',  ( 7.690461757479017101E-15, -129.2000000000000455, 0.000000000000000000 ) ) ;
#14367 = DIRECTION ( 'NONE',  ( 1.000000000000000000, 0.000000000000000000, -0.000000000000000000 ) ) ;
#14368 = PRODUCT_RELATED_PRODUCT_CATEGORY ( 'part', '', ( #23269 ) ) ;
#14369 = DIRECTION ( 'NONE',  ( -0.000000000000000000, -0.000000000000000000, 1.000000000000000000 ) ) ;
#14370 = CARTESIAN_POINT ( 'NONE',  ( -285.2000000000006708, 90.00000000000102318, -35.00000000000001421 ) ) ;
#14371 = DIRECTION ( 'NONE',  ( 0.000000000000000000, 0.000000000000000000, 1.000000000000000000 ) ) ;
#14372 = CARTESIAN_POINT ( 'NONE',  ( 3.272451888078290683, 24.83884780301428208, 145.0000120000000265 ) ) ;
#14373 = EDGE_LOOP ( 'NONE', ( #17670, #16236, #7496, #4874 ) ) ;
#14374 = VERTEX_POINT ( 'NONE', #8300 ) ;
#14375 = CARTESIAN_POINT ( 'NONE',  ( 44.80746418436846312, -137.9031948627969655, -90.00000000000000000 ) ) ;
#14376 = CARTESIAN_POINT ( 'NONE',  ( 90.00000000000000000, -149.9999999999996874, 129.9038105676659711 ) ) ;
#14377 = ORIENTED_EDGE ( 'NONE', *, *, #15780, .F. ) ;
#14378 = FACE_OUTER_BOUND ( 'NONE', #11855, .T. ) ;
#14379 = PLANE ( 'NONE',  #21122 ) ;
#14380 = ORIENTED_EDGE ( 'NONE', *, *, #21969, .T. ) ;
#14381 = DIRECTION ( 'NONE',  ( -0.000000000000000000, -0.000000000000000000, 1.000000000000000000 ) ) ;
#14382 = DIRECTION ( 'NONE',  ( -1.000000000000000000, 0.000000000000000000, 0.000000000000000000 ) ) ;
#14383 = ORIENTED_EDGE ( 'NONE', *, *, #8892, .T. ) ;
#14384 = PLANE ( 'NONE',  #2881 ) ;
#14385 = ORIENTED_EDGE ( 'NONE', *, *, #5363, .F. ) ;
#14386 = LINE ( 'NONE', #20019, #14967 ) ;
#14387 = CARTESIAN_POINT ( 'NONE',  ( -51.87806360044816500, 135.4018704341555974, -90.00000000000000000 ) ) ;
#14388 = ORIENTED_EDGE ( 'NONE', *, *, #23742, .F. ) ;
#14389 = VERTEX_POINT ( 'NONE', #6360 ) ;
#14390 = LINE ( 'NONE', #8815, #13926 ) ;
#14391 = CONICAL_SURFACE ( 'NONE', #1252, 2.055000000000001492, 0.7853981633974633780 ) ;
#14392 = DIRECTION ( 'NONE',  ( 6.123233995736766036E-17, 0.000000000000000000, -1.000000000000000000 ) ) ;
#14393 = CARTESIAN_POINT ( 'NONE',  ( -126.9531799701276213, 88.92639545932848932, -31.88829724122659570 ) ) ;
#14394 = EDGE_CURVE ( 'NONE', #10145, #22628, #15795, .T. ) ;
#14395 = EDGE_CURVE ( 'NONE', #10091, #10816, #4316, .T. ) ;
#14396 = DIRECTION ( 'NONE',  ( 0.000000000000000000, 0.000000000000000000, -1.000000000000000000 ) ) ;
#14397 = LINE ( 'NONE', #18224, #17858 ) ;
#14398 = ORIENTED_EDGE ( 'NONE', *, *, #3538, .T. ) ;
#14399 = CYLINDRICAL_SURFACE ( 'NONE', #21476, 7.500000000000000888 ) ;
#14400 = SHAPE_REPRESENTATION_RELATIONSHIP ( 'NONE' , 'NONE' ,  #6508, #16222 ) ;
#14401 = ORIENTED_EDGE ( 'NONE', *, *, #8549, .F. ) ;
#14402 = PLANE ( 'NONE',  #3659 ) ;
#14403 = CARTESIAN_POINT ( 'NONE',  ( 285.2000000000013529, -127.0000000000000568, -146.4928932188134070 ) ) ;
#14404 = EDGE_LOOP ( 'NONE', ( #7767, #19376, #4366, #23767 ) ) ;
#14405 = CYLINDRICAL_SURFACE ( 'NONE', #235, 7.500000000000007105 ) ;
#14406 = EDGE_LOOP ( 'NONE', ( #19945, #1204, #13511, #7882 ) ) ;
#14407 = DIRECTION ( 'NONE',  ( 0.000000000000000000, -0.8660254037844398178, -0.4999999999999980016 ) ) ;
#14408 = ORIENTED_EDGE ( 'NONE', *, *, #10982, .T. ) ;
#14409 = FACE_OUTER_BOUND ( 'NONE', #4030, .T. ) ;
#14410 = EDGE_CURVE ( 'NONE', #10909, #12392, #5370, .T. ) ;
#14411 = DIRECTION ( 'NONE',  ( -0.000000000000000000, -0.000000000000000000, 1.000000000000000000 ) ) ;
#14412 = DIRECTION ( 'NONE',  ( 0.000000000000000000, 0.4999999999999993894, -0.8660254037844389297 ) ) ;
#14413 = ADVANCED_FACE ( 'NONE', ( #8070 ), #5042, .F. ) ;
#14414 = DIRECTION ( 'NONE',  ( 0.000000000000000000, -0.000000000000000000, 1.000000000000000000 ) ) ;
#14415 = ORIENTED_EDGE ( 'NONE', *, *, #3626, .T. ) ;
#14416 = FACE_OUTER_BOUND ( 'NONE', #632, .T. ) ;
#14418 = ORIENTED_EDGE ( 'NONE', *, *, #7127, .T. ) ;
#14417 = ORIENTED_EDGE ( 'NONE', *, *, #22626, .T. ) ;
#14419 = CARTESIAN_POINT ( 'NONE',  ( 162.9999999999998010, -801.0618695410399823, 30.00000000000653699 ) ) ;
#14420 = DIRECTION ( 'NONE',  ( 0.000000000000000000, 0.000000000000000000, -1.000000000000000000 ) ) ;
#14421 = DIRECTION ( 'NONE',  ( -6.640089860198304064E-16, -1.000000000000000000, 3.495664435217746987E-15 ) ) ;
#14422 = VERTEX_POINT ( 'NONE', #12318 ) ;
#14423 = CIRCLE ( 'NONE', #17528, 2.649999999999999467 ) ;
#14424 = DIRECTION ( 'NONE',  ( 3.495664435217746987E-15, 1.000000000000000000, 0.000000000000000000 ) ) ;
#14425 = EDGE_LOOP ( 'NONE', ( #3051, #283, #3915, #5923 ) ) ;
#14426 = PLANE ( 'NONE',  #18393 ) ;
#14427 = VERTEX_POINT ( 'NONE', #21447 ) ;
#14428 = FACE_OUTER_BOUND ( 'NONE', #19627, .T. ) ;
#14429 = CARTESIAN_POINT ( 'NONE',  ( 0.000000000000000000, 0.000000000000000000, -5.000000000000000000 ) ) ;
#14430 = CONTEXT_DEPENDENT_SHAPE_REPRESENTATION ( #22200, #4472 ) ;
#14431 = ADVANCED_FACE ( 'NONE', ( #3195 ), #14357, .T. ) ;
#14432 = ORIENTED_EDGE ( 'NONE', *, *, #20078, .F. ) ;
#14433 = ORIENTED_EDGE ( 'NONE', *, *, #5471, .F. ) ;
#14434 = EDGE_CURVE ( 'NONE', #16240, #8499, #2699, .T. ) ;
#14435 = DIRECTION ( 'NONE',  ( 0.000000000000000000, 0.000000000000000000, 1.000000000000000000 ) ) ;
#14436 = VERTEX_POINT ( 'NONE', #19504 ) ;
#14437 = CARTESIAN_POINT ( 'NONE',  ( -109.8074641843675749, 85.22886158240835641, 90.00000000000000000 ) ) ;
#14438 = DIRECTION ( 'NONE',  ( 1.000000000000000000, 0.000000000000000000, 0.000000000000000000 ) ) ;
#14439 = VECTOR ( 'NONE', #4468, 1000.000000000000000 ) ;
#14440 = PRODUCT_DEFINITION_SHAPE ( 'NONE', 'NONE',  #20665 ) ;
#14441 = CIRCLE ( 'NONE', #3988, 160.0000000000000000 ) ;
#14442 = CARTESIAN_POINT ( 'NONE',  ( 2.500000000000000000, 0.000000000000000000, 0.000000000000000000 ) ) ;
#14443 = CARTESIAN_POINT ( 'NONE',  ( -146.4450000000005332, -784.4690652294799520, -29.99999999999356248 ) ) ;
#14444 = DIRECTION ( 'NONE',  ( 0.000000000000000000, 0.000000000000000000, 1.000000000000000000 ) ) ;
#14445 = ORIENTED_EDGE ( 'NONE', *, *, #17653, .T. ) ;
#14446 = CARTESIAN_POINT ( 'NONE',  ( 0.000000000000000000, 1.178949249685213863, -2.042000000000001148 ) ) ;
#14447 = CARTESIAN_POINT ( 'NONE',  ( -3.522875095019672109, 2.820352903225427532, -3.598441714920591394 ) ) ;
#14448 = ADVANCED_FACE ( 'NONE', ( #6721, #2954, #3319, #8913, #17829, #16142, #23506, #21330, #1397 ), #16375, .T. ) ;
#14449 = ORIENTED_EDGE ( 'NONE', *, *, #12685, .F. ) ;
#14450 = LINE ( 'NONE', #22134, #20808 ) ;
#14451 = DIRECTION ( 'NONE',  ( 0.8660254037844381525, -0.5000000000000007772, 0.000000000000000000 ) ) ;
#14452 = CARTESIAN_POINT ( 'NONE',  ( 155.0000000000000568, -801.0618695410406644, -29.99999999999350564 ) ) ;
#14453 = VECTOR ( 'NONE', #19255, 1000.000000000000000 ) ;
#14454 = DIRECTION ( 'NONE',  ( 1.000000000000000000, 0.000000000000000000, 0.000000000000000000 ) ) ;
#14455 = CARTESIAN_POINT ( 'NONE',  ( 281.1810844504668125, 269.4795879751484904, -149.9329465209279704 ) ) ;
#14456 = AXIS2_PLACEMENT_3D ( 'NONE', #16173, #12699, #21711 ) ;
#14457 = ORIENTED_EDGE ( 'NONE', *, *, #871, .F. ) ;
#14458 = CARTESIAN_POINT ( 'NONE',  ( 155.0000000000000568, -801.0618695410406644, -29.99999999999350564 ) ) ;
#14459 = ORIENTED_EDGE ( 'NONE', *, *, #901, .F. ) ;
#14460 = DIRECTION ( 'NONE',  ( -1.000000000000000000, 0.000000000000000000, 0.000000000000000000 ) ) ;
#14461 = FACE_OUTER_BOUND ( 'NONE', #2372, .T. ) ;
#14462 = ORIENTED_EDGE ( 'NONE', *, *, #4184, .T. ) ;
#14463 =( NAMED_UNIT ( * ) SI_UNIT ( $, .STERADIAN. ) SOLID_ANGLE_UNIT ( ) );
#14464 = DIRECTION ( 'NONE',  ( 0.000000000000000000, 0.000000000000000000, -1.000000000000000000 ) ) ;
#14465 = ADVANCED_FACE ( 'NONE', ( #21688 ), #23612, .T. ) ;
#14466 = FACE_OUTER_BOUND ( 'NONE', #18889, .T. ) ;
#14467 = EDGE_CURVE ( 'NONE', #4130, #14975, #9261, .T. ) ;
#14468 = DIRECTION ( 'NONE',  ( 0.000000000000000000, 0.000000000000000000, -1.000000000000000000 ) ) ;
#14469 = CARTESIAN_POINT ( 'NONE',  ( 50.00000000000000000, 4.171999999999999709, 0.000000000000000000 ) ) ;
#14470 = CARTESIAN_POINT ( 'NONE',  ( 15.24974479720505549, 19.87769063953887283, 145.0000119999999697 ) ) ;
#14471 = ORIENTED_EDGE ( 'NONE', *, *, #16202, .F. ) ;
#14472 = CIRCLE ( 'NONE', #21732, 5.249999999999962697 ) ;
#14473 = ORIENTED_EDGE ( 'NONE', *, *, #4495, .T. ) ;
#14474 = DIRECTION ( 'NONE',  ( 1.000000000000000000, 0.000000000000000000, 0.000000000000000000 ) ) ;
#14475 = CARTESIAN_POINT ( 'NONE',  ( -64.99999999999998579, -56.79999999999943583, 125.0000000000001705 ) ) ;
#14476 = ADVANCED_FACE ( 'NONE', ( #5143 ), #12761, .F. ) ;
#14477 = ORIENTED_EDGE ( 'NONE', *, *, #1862, .T. ) ;
#14478 = AXIS2_PLACEMENT_3D ( 'NONE', #1581, #22081, #5555 ) ;
#14479 = EDGE_CURVE ( 'NONE', #4882, #19949, #3843, .T. ) ;
#14480 = AXIS2_PLACEMENT_3D ( 'NONE', #18656, #20718, #14956 ) ;
#14481 = FACE_OUTER_BOUND ( 'NONE', #15636, .T. ) ;
#14482 = CARTESIAN_POINT ( 'NONE',  ( -79.99999999999995737, -56.79999999999918714, 250.0000000000000000 ) ) ;
#14483 = EDGE_LOOP ( 'NONE', ( #19837, #1014 ) ) ;
#14484 = CYLINDRICAL_SURFACE ( 'NONE', #23685, 5.199999999999982414 ) ;
#14485 = CARTESIAN_POINT ( 'NONE',  ( 2.452879891156805492, 7.244083172395185954, -0.1007566405101774504 ) ) ;
#14486 = ORIENTED_EDGE ( 'NONE', *, *, #19719, .F. ) ;
#14487 = DIRECTION ( 'NONE',  ( 0.000000000000000000, 0.000000000000000000, 1.000000000000000000 ) ) ;
#14488 = AXIS2_PLACEMENT_3D ( 'NONE', #3579, #9289, #5644 ) ;
#14489 = VERTEX_POINT ( 'NONE', #3093 ) ;
#14490 = CYLINDRICAL_SURFACE ( 'NONE', #1444, 7.500000000000000000 ) ;
#14491 = CARTESIAN_POINT ( 'NONE',  ( 0.000000000000000000, -1.178949249685215417, 2.042000000000002036 ) ) ;
#14492 = ORIENTED_EDGE ( 'NONE', *, *, #2033, .T. ) ;
#14493 = ORIENTED_EDGE ( 'NONE', *, *, #15516, .T. ) ;
#14494 = CARTESIAN_POINT ( 'NONE',  ( 285.2299999999999045, 267.7999999999999545, -146.4928932188133786 ) ) ;
#14495 = VECTOR ( 'NONE', #11217, 1000.000000000000000 ) ;
#14496 = CLOSED_SHELL ( 'NONE', ( #11580, #9137, #6321, #19449, #8547, #8936, #5163, #22400, #13182, #7565, #10164, #18254, #14022, #16278, #22669, #6598, #16540, #17438, #18298, #13464, #6399, #7613, #11686, #11262, #5865, #15043, #22562, #15206, #19195, #15675, #21723, #19023 ) ) ;
#14497 = CARTESIAN_POINT ( 'NONE',  ( -126.6052862049306924, 89.42094583968793131, -31.11320915316591851 ) ) ;
#14498 = DIRECTION ( 'NONE',  ( -0.000000000000000000, -0.000000000000000000, 1.000000000000000000 ) ) ;
#14499 = FACE_BOUND ( 'NONE', #2867, .T. ) ;
#14500 = EDGE_LOOP ( 'NONE', ( #14625, #12448, #18521, #16118 ) ) ;
#14501 = EDGE_CURVE ( 'NONE', #17898, #7277, #18065, .T. ) ;
#14502 = DIRECTION ( 'NONE',  ( -0.000000000000000000, 0.000000000000000000, 1.000000000000000000 ) ) ;
#14503 = AXIS2_PLACEMENT_3D ( 'NONE', #23008, #19750, #21332 ) ;
#14504 =( NAMED_UNIT ( * ) SI_UNIT ( $, .STERADIAN. ) SOLID_ANGLE_UNIT ( ) );
#14505 = EDGE_CURVE ( 'NONE', #21432, #16240, #1168, .T. ) ;
#14506 = EDGE_CURVE ( 'NONE', #2113, #23382, #8111, .T. ) ;
#14507 = VECTOR ( 'NONE', #1579, 1000.000000000000000 ) ;
#14508 = ADVANCED_FACE ( 'NONE', ( #21576 ), #1629, .T. ) ;
#14509 = VECTOR ( 'NONE', #2072, 1000.000000000000114 ) ;
#14510 = CARTESIAN_POINT ( 'NONE',  ( 235.0000000000000284, -560.0000000000000000, -60.00000000000000711 ) ) ;
#14511 = CARTESIAN_POINT ( 'NONE',  ( 91.18044947428789726, 112.7436279071541776, 90.00000000000000000 ) ) ;
#14512 = EDGE_CURVE ( 'NONE', #3355, #12111, #8542, .T. ) ;
#14513 = ORIENTED_EDGE ( 'NONE', *, *, #20938, .F. ) ;
#14515 = EDGE_CURVE ( 'NONE', #422, #15468, #15912, .T. ) ;
#14514 = CARTESIAN_POINT ( 'NONE',  ( 160.0000000000000000, 1.959434878635765210E-14, 100.0000000000000000 ) ) ;
#14516 = ORIENTED_EDGE ( 'NONE', *, *, #23640, .F. ) ;
#14517 = CIRCLE ( 'NONE', #12221, 7.500000000000000888 ) ;
#14518 = CARTESIAN_POINT ( 'NONE',  ( 0.000000000000000000, 0.000000000000000000, 4.000000000000000000 ) ) ;
#14519 = EDGE_LOOP ( 'NONE', ( #12541, #20998 ) ) ;
#14520 = CARTESIAN_POINT ( 'NONE',  ( -287.4000000000014552, -132.2000000000000455, -146.4928932188134070 ) ) ;
#14521 = CARTESIAN_POINT ( 'NONE',  ( -24.99999999999998224, -1001.636246173744439, 145.0000119999999697 ) ) ;
#14522 = DIRECTION ( 'NONE',  ( 0.7232617928448825673, -0.6905739489807055653, -6.982962677686266711E-15 ) ) ;
#14523 = CARTESIAN_POINT ( 'NONE',  ( -137.9031948627974486, 44.80746418436699940, -90.00000000000000000 ) ) ;
#14524 = EDGE_CURVE ( 'NONE', #19753, #18149, #14020, .T. ) ;
#14525 = LINE ( 'NONE', #4979, #2657 ) ;
#14526 = ORIENTED_EDGE ( 'NONE', *, *, #12769, .T. ) ;
#14527 = CARTESIAN_POINT ( 'NONE',  ( 70.00000000000000000, -87.33333333333332860, 0.000000000000000000 ) ) ;
#14528 = SURFACE_SIDE_STYLE ('',( #23678 ) ) ;
#14530 = ORIENTED_EDGE ( 'NONE', *, *, #15687, .F. ) ;
#14529 = ORIENTED_EDGE ( 'NONE', *, *, #12630, .T. ) ;
#14531 = DIRECTION ( 'NONE',  ( 1.224646799147353207E-16, -4.064521778635712183E-50, -1.000000000000000000 ) ) ;
#14532 = CARTESIAN_POINT ( 'NONE',  ( -2.700000000000001510, 3.024877593893962577E-15, 24.69999999999999929 ) ) ;
#14533 = CIRCLE ( 'NONE', #7566, 2.649999999999985700 ) ;
#14534 = CARTESIAN_POINT ( 'NONE',  ( 4.000000000000000888, 1.563622288139206118, -0.2253451193528334950 ) ) ;
#14535 = ORIENTED_EDGE ( 'NONE', *, *, #2806, .F. ) ;
#14536 = DIRECTION ( 'NONE',  ( 1.000000000000000000, 0.000000000000000000, -0.000000000000000000 ) ) ;
#14537 = EDGE_CURVE ( 'NONE', #16635, #9210, #3580, .T. ) ;
#14538 = CIRCLE ( 'NONE', #17604, 20.00000000000001776 ) ;
#14539 = EDGE_CURVE ( 'NONE', #9973, #2882, #17728, .T. ) ;
#14540 = DIRECTION ( 'NONE',  ( 0.000000000000000000, 0.000000000000000000, 1.000000000000000000 ) ) ;
#14541 = ORIENTED_EDGE ( 'NONE', *, *, #4099, .T. ) ;
#14542 = DIRECTION ( 'NONE',  ( 5.758888509154132365E-17, 0.7071067811865489050, 0.7071067811865462405 ) ) ;
#14543 = AXIS2_PLACEMENT_3D ( 'NONE', #10285, #17873, #21735 ) ;
#14544 = ORIENTED_EDGE ( 'NONE', *, *, #8900, .F. ) ;
#14545 = ORIENTED_EDGE ( 'NONE', *, *, #15493, .T. ) ;
#14546 = DIRECTION ( 'NONE',  ( 0.000000000000000000, 0.000000000000000000, 1.000000000000000000 ) ) ;
#14547 = ORIENTED_EDGE ( 'NONE', *, *, #21980, .T. ) ;
#14548 = CONICAL_SURFACE ( 'NONE', #4105, 7.500000000000001776, 0.8594454914424796144 ) ;
#14549 = LINE ( 'NONE', #10832, #4367 ) ;
#14550 = CARTESIAN_POINT ( 'NONE',  ( 133.9566469371582684, 77.97836475581249260, 28.74044610054856008 ) ) ;
#14551 = DIRECTION ( 'NONE',  ( 0.000000000000000000, -1.000000000000000000, 0.000000000000000000 ) ) ;
#14552 = CARTESIAN_POINT ( 'NONE',  ( 35.00000000000000711, -3.880967142342036772E-28, -150.2000000000008981 ) ) ;
#14553 = FACE_OUTER_BOUND ( 'NONE', #7466, .T. ) ;
#14554 = EDGE_LOOP ( 'NONE', ( #10641, #23102, #2510, #15172 ) ) ;
#14555 = SURFACE_STYLE_FILL_AREA ( #8999 ) ;
#14556 = CARTESIAN_POINT ( 'NONE',  ( 235.0000000000000284, -489.9999999999998863, 60.00000000000000000 ) ) ;
#14557 = DIRECTION ( 'NONE',  ( 1.000000000000000000, 0.000000000000000000, 0.000000000000000000 ) ) ;
#14558 = AXIS2_PLACEMENT_3D ( 'NONE', #15813, #17966, #6491 ) ;
#14559 =( BOUNDED_SURFACE ( )  B_SPLINE_SURFACE ( 3, 2, ( 
 ( #14051, #8712, #21381 ),
 ( #4840, #3013, #10425 ),
 ( #17775, #1220, #8592 ),
 ( #18002, #23306, #14167 ),
 ( #21636, #1449, #16427 ),
 ( #5443, #12729, #19923 ),
 ( #23780, #14623, #9423 ),
 ( #13082, #3372, #20048 ) ),
 .UNSPECIFIED., .F., .F., .F. ) 
 B_SPLINE_SURFACE_WITH_KNOTS ( ( 4, 2, 2, 4 ),
 ( 3, 3 ),
 ( 0.03861844051980969222, 0.04325213341840641185, 0.04556897986770477166, 0.04788582631700313147 ),
 ( 0.000000000000000000, 1.000000000000000000 ),
 .UNSPECIFIED. ) 
 GEOMETRIC_REPRESENTATION_ITEM ( )  RATIONAL_B_SPLINE_SURFACE ( (
 ( 1.000000000000000000, 0.8047781759831921233, 1.000000000000000000),
 ( 1.000000000000000000, 0.8123762462806503049, 1.000000000000000000),
 ( 1.000000000000000000, 0.8190659850614813164, 1.000000000000000000),
 ( 1.000000000000000000, 0.8191937571014595854, 1.000000000000000000),
 ( 1.000000000000000000, 0.8176092952779865364, 1.000000000000000000),
 ( 1.000000000000000000, 0.8122962088597069918, 1.000000000000000000),
 ( 1.000000000000000000, 0.8086311330827506971, 1.000000000000000000),
 ( 1.000000000000000000, 0.8047712282214323221, 1.000000000000000000) ) ) 
 REPRESENTATION_ITEM ( '' )  SURFACE ( )  );
#14560 = VERTEX_POINT ( 'NONE', #15929 ) ;
#14561 = CARTESIAN_POINT ( 'NONE',  ( 280.9954397628184779, 268.9021437883073986, -146.9094021484633856 ) ) ;
#14562 = FACE_OUTER_BOUND ( 'NONE', #11235, .T. ) ;
#14563 = VECTOR ( 'NONE', #6746, 1000.000000000000000 ) ;
#14564 = CIRCLE ( 'NONE', #10739, 2.649999999999985700 ) ;
#14565 = DIRECTION ( 'NONE',  ( 1.000000000000000000, -3.495664435217746987E-15, -0.000000000000000000 ) ) ;
#14566 = CARTESIAN_POINT ( 'NONE',  ( -72.64999999999996305, -112.6666666666667140, 148.0000000000000000 ) ) ;
#14567 = CARTESIAN_POINT ( 'NONE',  ( 280.4358181722191148, 272.4728700860325148, -147.3062614524586138 ) ) ;
#14568 = ORIENTED_EDGE ( 'NONE', *, *, #5050, .T. ) ;
#14569 = CARTESIAN_POINT ( 'NONE',  ( 0.000000000000000000, 0.000000000000000000, -50.00000000000000000 ) ) ;
#14570 = ORIENTED_EDGE ( 'NONE', *, *, #1150, .F. ) ;
#14571 = CARTESIAN_POINT ( 'NONE',  ( 21.00000000000000355, 2.789133085058097101E-16, -2.055000000000000160 ) ) ;
#14572 = VERTEX_POINT ( 'NONE', #2859 ) ;
#14573 = VECTOR ( 'NONE', #13648, 1000.000000000000000 ) ;
#14574 =( NAMED_UNIT ( * ) PLANE_ANGLE_UNIT ( ) SI_UNIT ( $, .RADIAN. ) );
#14575 = CARTESIAN_POINT ( 'NONE',  ( 123.2641556675335437, -1093.973169342143592, -31.53250949154602623 ) ) ;
#14576 = FACE_BOUND ( 'NONE', #14953, .T. ) ;
#14577 = CARTESIAN_POINT ( 'NONE',  ( 22.46869086670261950, -1011.084058742425668, -145.0000000000001137 ) ) ;
#14579 = AXIS2_PLACEMENT_3D ( 'NONE', #8981, #9343, #14326 ) ;
#14578 = CARTESIAN_POINT ( 'NONE',  ( -2.352990130084580066E-16, 8.660254037844390851, -10.00000000000000000 ) ) ;
#14580 = CYLINDRICAL_SURFACE ( 'NONE', #6897, 5.249999999999942268 ) ;
#14581 = CARTESIAN_POINT ( 'NONE',  ( -16.52066876451830524, 18.83467029480907584, 145.0000119999999697 ) ) ;
#14582 = AXIS2_PLACEMENT_3D ( 'NONE', #16448, #8737, #15986 ) ;
#14583 = ORIENTED_EDGE ( 'NONE', *, *, #4904, .T. ) ;
#14584 = ORIENTED_EDGE ( 'NONE', *, *, #10769, .F. ) ;
#14585 = DIRECTION ( 'NONE',  ( -0.000000000000000000, -1.177509268541832635E-16, 1.000000000000000000 ) ) ;
#14586 = DIRECTION ( 'NONE',  ( 0.000000000000000000, 0.000000000000000000, -1.000000000000000000 ) ) ;
#14587 = ORIENTED_EDGE ( 'NONE', *, *, #22227, .T. ) ;
#14588 = DIRECTION ( 'NONE',  ( 1.000000000000000000, -0.000000000000000000, -0.000000000000000000 ) ) ;
#14589 = CARTESIAN_POINT ( 'NONE',  ( 6.486836893983020325, -4.915077010914103539, -7.231838333420563814 ) ) ;
#14590 = ORIENTED_EDGE ( 'NONE', *, *, #19, .T. ) ;
#14591 = LINE ( 'NONE', #21939, #168 ) ;
#14592 = EDGE_CURVE ( 'NONE', #22764, #17672, #1910, .T. ) ;
#14593 = CARTESIAN_POINT ( 'NONE',  ( 72.64999999999999147, -112.6666666666666714, 124.9999999999999858 ) ) ;
#14594 = ORIENTED_EDGE ( 'NONE', *, *, #18012, .F. ) ;
#14595 = AXIS2_PLACEMENT_3D ( 'NONE', #13834, #10303, #15974 ) ;
#14596 = CARTESIAN_POINT ( 'NONE',  ( -2.352990130084580066E-16, 8.660254037844390851, -7.422398894150034288 ) ) ;
#14597 = EDGE_CURVE ( 'NONE', #22831, #19928, #8315, .T. ) ;
#14598 = DIRECTION ( 'NONE',  ( 0.000000000000000000, 0.000000000000000000, -1.000000000000000000 ) ) ;
#14599 = EDGE_CURVE ( 'NONE', #12943, #23173, #10144, .T. ) ;
#14600 = AXIS2_PLACEMENT_3D ( 'NONE', #7433, #5395, #3456 ) ;
#14601 = VERTEX_POINT ( 'NONE', #8207 ) ;
#14602 = CARTESIAN_POINT ( 'NONE',  ( 7.922281120364393914, 4.573931137438269623, -8.047472243342930653 ) ) ;
#14603 = DIRECTION ( 'NONE',  ( 0.000000000000000000, -1.000000000000000000, 0.000000000000000000 ) ) ;
#14604 = EDGE_CURVE ( 'NONE', #10884, #6133, #1054, .T. ) ;
#14605 = CARTESIAN_POINT ( 'NONE',  ( -85.22886158240879695, 117.3074641843673049, -90.00000000000000000 ) ) ;
#14606 = ORIENTED_EDGE ( 'NONE', *, *, #12558, .T. ) ;
#14607 = ORIENTED_EDGE ( 'NONE', *, *, #17831, .T. ) ;
#14608 = CARTESIAN_POINT ( 'NONE',  ( -146.4450000000005332, -204.4690652294800657, -29.99999999999356248 ) ) ;
#14609 = SHAPE_DEFINITION_REPRESENTATION ( #3420, #14711 ) ;
#14610 = CARTESIAN_POINT ( 'NONE',  ( -127.9021285790837510, 87.55595642181940264, -27.49999999999351985 ) ) ;
#14611 = CARTESIAN_POINT ( 'NONE',  ( 124.4701338314433201, -1092.369831568443260, -32.49999999999351985 ) ) ;
#14612 = LINE ( 'NONE', #3592, #2016 ) ;
#14613 = AXIS2_PLACEMENT_3D ( 'NONE', #1779, #5784, #12713 ) ;
#14614 = ORIENTED_EDGE ( 'NONE', *, *, #1758, .F. ) ;
#14615 = AXIS2_PLACEMENT_3D ( 'NONE', #10978, #12815, #85 ) ;
#14616 = DIRECTION ( 'NONE',  ( 0.000000000000000000, -1.000000000000000000, 0.000000000000000000 ) ) ;
#14617 = AXIS2_PLACEMENT_3D ( 'NONE', #9234, #5595, #3419 ) ;
#14618 = AXIS2_PLACEMENT_3D ( 'NONE', #21158, #15513, #15271 ) ;
#14619 = AXIS2_PLACEMENT_3D ( 'NONE', #19751, #3199, #21333 ) ;
#14620 = DIRECTION ( 'NONE',  ( 0.000000000000000000, 1.000000000000000000, 0.000000000000000000 ) ) ;
#14621 = CARTESIAN_POINT ( 'NONE',  ( 1.500000000000000000, 11.99999999999999822, 200.2421591959677016 ) ) ;
#14622 = ORIENTED_EDGE ( 'NONE', *, *, #22528, .F. ) ;
#14623 = CARTESIAN_POINT ( 'NONE',  ( 0.3875187462248268488, 8.436519985393664101, -7.781689322726965230 ) ) ;
#14624 = EDGE_CURVE ( 'NONE', #7615, #21317, #764, .T. ) ;
#14625 = ORIENTED_EDGE ( 'NONE', *, *, #7377, .F. ) ;
#14626 = PRODUCT_DEFINITION_SHAPE ( 'NONE', 'NONE',  #16837 ) ;
#14627 =( GEOMETRIC_REPRESENTATION_CONTEXT ( 3 ) GLOBAL_UNCERTAINTY_ASSIGNED_CONTEXT ( ( #22948 ) ) GLOBAL_UNIT_ASSIGNED_CONTEXT ( ( #10972, #14574, #20220 ) ) REPRESENTATION_CONTEXT ( 'NONE', 'WORKASPACE' ) );
#14629 = TOROIDAL_SURFACE ( 'NONE', #738, 20.30000000000000071, 0.3000000000000059841 ) ;
#14628 = PRESENTATION_LAYER_ASSIGNMENT (  '', '', ( #16550 ) ) ;
#14630 = CIRCLE ( 'NONE', #20783, 7.500000000000005329 ) ;
#14632 = CARTESIAN_POINT ( 'NONE',  ( 0.000000000000000000, 0.000000000000000000, -150.0000000000000000 ) ) ;
#14631 = AXIS2_PLACEMENT_3D ( 'NONE', #9499, #4033, #16850 ) ;
#14633 = EDGE_CURVE ( 'NONE', #22322, #8986, #22873, .T. ) ;
#14634 = AXIS2_PLACEMENT_3D ( 'NONE', #23155, #6620, #15688 ) ;
#14635 = CARTESIAN_POINT ( 'NONE',  ( -1.287237434361707233, -3.875615274277397937, -3.430618716626816500 ) ) ;
#14636 = VERTEX_POINT ( 'NONE', #21347 ) ;
#14637 = AXIS2_PLACEMENT_3D ( 'NONE', #7749, #22458, #1694 ) ;
#14638 = EDGE_CURVE ( 'NONE', #1322, #16743, #12218, .T. ) ;
#14639 = CARTESIAN_POINT ( 'NONE',  ( -105.0000000000000142, 30.00000000000001421, 3.000000000000000000 ) ) ;
#14640 = CARTESIAN_POINT ( 'NONE',  ( -19.87769063953884441, -1015.249744797204812, 145.0000119999999981 ) ) ;
#14641 = LINE ( 'NONE', #19697, #22290 ) ;
#14642 =( REPRESENTATION_RELATIONSHIP ('NONE','NONE', #10127, #8987 ) REPRESENTATION_RELATIONSHIP_WITH_TRANSFORMATION ( #17549 )SHAPE_REPRESENTATION_RELATIONSHIP( ) );
#14643 = DIRECTION ( 'NONE',  ( -0.000000000000000000, -0.000000000000000000, 1.000000000000000000 ) ) ;
#14644 = EDGE_CURVE ( 'NONE', #6149, #4706, #19272, .T. ) ;
#14645 = PRODUCT_DEFINITION ( 'UNKNOWN', '', #4237, #362 ) ;
#14646 = CIRCLE ( 'NONE', #20826, 2.199999999999979750 ) ;
#14647 = CARTESIAN_POINT ( 'NONE',  ( 89.00000000000000000, -74.99999999999998579, 3.000000000000000000 ) ) ;
#14648 = ORIENTED_EDGE ( 'NONE', *, *, #23777, .F. ) ;
#14649 = DIRECTION ( 'NONE',  ( -1.000000000000000000, 0.000000000000000000, 0.000000000000000000 ) ) ;
#14651 = EDGE_LOOP ( 'NONE', ( #10499, #18085, #14333, #14432 ) ) ;
#14650 = VERTEX_POINT ( 'NONE', #1187 ) ;
#14652 = DIRECTION ( 'NONE',  ( 0.9237280213470682178, 0.3830490080632377725, 1.131240564625405124E-16 ) ) ;
#14654 = AXIS2_PLACEMENT_3D ( 'NONE', #16556, #20275, #1932 ) ;
#14653 = AXIS2_PLACEMENT_3D ( 'NONE', #4740, #10452, #10686 ) ;
#14655 = FACE_OUTER_BOUND ( 'NONE', #12654, .T. ) ;
#14656 = CARTESIAN_POINT ( 'NONE',  ( 4.000000000000000000, 2.309401076758515803, -0.4999999999999995559 ) ) ;
#14657 = CIRCLE ( 'NONE', #35, 2.041999999999999815 ) ;
#14658 = VECTOR ( 'NONE', #2705, 1000.000000000000000 ) ;
#14659 = CIRCLE ( 'NONE', #8887, 2.500000000000002220 ) ;
#14660 = ORIENTED_EDGE ( 'NONE', *, *, #16709, .F. ) ;
#14661 = CYLINDRICAL_SURFACE ( 'NONE', #7957, 21.50000000000000000 ) ;
#14662 = AXIS2_PLACEMENT_3D ( 'NONE', #13601, #16758, #13057 ) ;
#14663 = DIRECTION ( 'NONE',  ( -4.183096374613631247E-18, 1.000000000000000000, 0.000000000000000000 ) ) ;
#14664 = VERTEX_POINT ( 'NONE', #8562 ) ;
#14665 = FACE_BOUND ( 'NONE', #11301, .T. ) ;
#14666 = CARTESIAN_POINT ( 'NONE',  ( 1.567478505476134606E-15, 4.618802153517012066, -3.433295621305382905 ) ) ;
#14667 = ITEM_DEFINED_TRANSFORMATION ( 'NONE', 'NONE', #12020,  #11210 ) ;
#14668 = ORIENTED_EDGE ( 'NONE', *, *, #14908, .F. ) ;
#14669 = VERTEX_POINT ( 'NONE', #1294 ) ;
#14670 = CARTESIAN_POINT ( 'NONE',  ( 125.3881179880848293, -1091.120112697373088, 32.00444854364510405 ) ) ;
#14671 = AXIS2_PLACEMENT_3D ( 'NONE', #1702, #7387, #8973 ) ;
#14672 = ORIENTED_EDGE ( 'NONE', *, *, #11731, .T. ) ;
#14674 = AXIS2_PLACEMENT_3D ( 'NONE', #10296, #2893, #17520 ) ;
#14673 = CARTESIAN_POINT ( 'NONE',  ( -129.2722218393576554, 85.52013646629063714, 30.65375098132849274 ) ) ;
#14675 = STYLED_ITEM ( 'NONE', ( #285 ), #11926 ) ;
#14676 = CIRCLE ( 'NONE', #2697, 2.649999999999985700 ) ;
#14677 = DIRECTION ( 'NONE',  ( 1.000000000000000000, -0.000000000000000000, -0.000000000000000000 ) ) ;
#14678 = AXIS2_PLACEMENT_3D ( 'NONE', #15234, #17039, #11878 ) ;
#14679 = VECTOR ( 'NONE', #14103, 1000.000000000000000 ) ;
#14680 = CARTESIAN_POINT ( 'NONE',  ( 44.80746418436557832, 137.9031948627978750, -90.00000000000000000 ) ) ;
#14681 = EDGE_CURVE ( 'NONE', #15889, #9157, #14659, .T. ) ;
#14682 = EDGE_CURVE ( 'NONE', #19104, #13591, #22908, .T. ) ;
#14683 = FACE_OUTER_BOUND ( 'NONE', #11510, .T. ) ;
#14684 = EDGE_CURVE ( 'NONE', #23301, #17463, #21108, .T. ) ;
#14685 = CARTESIAN_POINT ( 'NONE',  ( 57.99999999999999289, -56.79999999999974136, 75.17098115668787273 ) ) ;
#14686 = ORIENTED_EDGE ( 'NONE', *, *, #1897, .F. ) ;
#14687 =( NAMED_UNIT ( * ) PLANE_ANGLE_UNIT ( ) SI_UNIT ( $, .RADIAN. ) );
#14688 = CARTESIAN_POINT ( 'NONE',  ( -51.87806360044718446, -135.4018704341559953, -90.00000000000000000 ) ) ;
#14689 = CARTESIAN_POINT ( 'NONE',  ( 281.4928932188134354, 267.8000000000000114, -144.9999999999999716 ) ) ;
#14690 = ORIENTED_EDGE ( 'NONE', *, *, #1212, .F. ) ;
#14691 = CARTESIAN_POINT ( 'NONE',  ( 0.000000000000000000, 0.000000000000000000, -4.000000000000000000 ) ) ;
#14692 = DIRECTION ( 'NONE',  ( 1.350636282998972974E-14, 0.000000000000000000, -1.000000000000000000 ) ) ;
#14693 = ORIENTED_EDGE ( 'NONE', *, *, #11821, .F. ) ;
#14694 = VECTOR ( 'NONE', #1433, 1000.000000000000000 ) ;
#14695 = CARTESIAN_POINT ( 'NONE',  ( -282.1427398886704054, 268.3758453455903918, 146.2440776823445105 ) ) ;
#14696 = CIRCLE ( 'NONE', #13949, 4.000000000000000000 ) ;
#14697 = LINE ( 'NONE', #7066, #8418 ) ;
#14698 = LINE ( 'NONE', #13020, #23115 ) ;
#14699 = VERTEX_POINT ( 'NONE', #3807 ) ;
#14700 = DIRECTION ( 'NONE',  ( 0.000000000000000000, 0.000000000000000000, -1.000000000000000000 ) ) ;
#14701 = VERTEX_POINT ( 'NONE', #20001 ) ;
#14702 = CARTESIAN_POINT ( 'NONE',  ( -4.000000000000000888, -1.539600717839011201, -3.300726591567081591 ) ) ;
#14703 = CARTESIAN_POINT ( 'NONE',  ( -146.0000000000005400, -784.4690652294799520, -32.05499999999356930 ) ) ;
#14704 = EDGE_LOOP ( 'NONE', ( #6015, #20046, #7375, #22810 ) ) ;
#14705 = CARTESIAN_POINT ( 'NONE',  ( 124.4701338314433485, -1092.369831568443260, -27.49999999999351985 ) ) ;
#14706 = FACE_BOUND ( 'NONE', #14274, .T. ) ;
#14707 = CARTESIAN_POINT ( 'NONE',  ( 24.19933745023729443, -1006.487655866706632, -145.0000000000001137 ) ) ;
#14708 = DIRECTION ( 'NONE',  ( 1.000000000000000000, 0.000000000000000000, 0.000000000000000000 ) ) ;
#14709 = CARTESIAN_POINT ( 'NONE',  ( 232.0000000000000284, 6.439293542825908723E-15, 0.000000000000000000 ) ) ;
#14710 = CARTESIAN_POINT ( 'NONE',  ( -3.272451888078327098, 24.83884780301426787, 145.0000119999999697 ) ) ;
#14711 = SHAPE_REPRESENTATION ( 'angular contact ball bearing_68_iso_ISO 15 ABB - 1740 - 38,SI,NC,38_68', ( #11210 ), #9278 ) ;
#14712 = EDGE_CURVE ( 'NONE', #15457, #52, #16390, .T. ) ;
#14713 = VERTEX_POINT ( 'NONE', #12692 ) ;
#14714 = ORIENTED_EDGE ( 'NONE', *, *, #12004, .T. ) ;
#14715 = CARTESIAN_POINT ( 'NONE',  ( 0.6507732100473444525, -4.243078065514795050, -0.2236248678334952777 ) ) ;
#14716 = DIRECTION ( 'NONE',  ( 1.000000000000000000, 0.000000000000000000, 0.000000000000000000 ) ) ;
#14717 = VERTEX_POINT ( 'NONE', #16505 ) ;
#14718 = DIRECTION ( 'NONE',  ( 0.6568457881071649851, 0.2618274444092050790, 0.7071067811865631159 ) ) ;
#14719 = CARTESIAN_POINT ( 'NONE',  ( 0.000000000000000000, 0.000000000000000000, 100.0000000000000000 ) ) ;
#14720 = VERTEX_POINT ( 'NONE', #7329 ) ;
#14721 = CARTESIAN_POINT ( 'NONE',  ( 281.3684665762323789, 268.0840560642351988, 147.1696999999999775 ) ) ;
#14723 = CARTESIAN_POINT ( 'NONE',  ( -0.6666666666666651864, 4.233901974057260098, -3.300726591567081147 ) ) ;
#14722 = B_SPLINE_CURVE_WITH_KNOTS ( 'NONE', 3,
 ( #6198, #11668, #18511, #162, #13483, #18973, #2439, #9829, #18857 ),
 .UNSPECIFIED., .F., .F.,
 ( 4, 2, 1, 2, 4 ),
 ( 0.000000000000000000, 0.002165063509461097498, 0.004330127018922194995, 0.006495190528383292493, 0.008660254037844389990 ),
 .UNSPECIFIED. ) ;
#14724 = ORIENTED_EDGE ( 'NONE', *, *, #787, .T. ) ;
#14725 = FACE_OUTER_BOUND ( 'NONE', #7414, .T. ) ;
#14726 = CARTESIAN_POINT ( 'NONE',  ( -4.000000000000000888, 1.563622288139195238, -0.2253451193528307472 ) ) ;
#14727 = DIRECTION ( 'NONE',  ( 0.000000000000000000, 0.000000000000000000, 1.000000000000000000 ) ) ;
#14728 = ORIENTED_EDGE ( 'NONE', *, *, #19191, .T. ) ;
#14729 = LINE ( 'NONE', #3699, #8795 ) ;
#14730 = CARTESIAN_POINT ( 'NONE',  ( 45.00000000000002132, -56.79999999999934346, 142.6500000000002046 ) ) ;
#14731 = CARTESIAN_POINT ( 'NONE',  ( 65.00000000000001421, -52.79999999999938609, 125.0000000000002274 ) ) ;
#14732 = ORIENTED_EDGE ( 'NONE', *, *, #1190, .F. ) ;
#14733 = VERTEX_POINT ( 'NONE', #5512 ) ;
#14734 = EDGE_CURVE ( 'NONE', #22784, #9608, #15447, .T. ) ;
#14735 = DIRECTION ( 'NONE',  ( -1.110223024625157172E-14, 0.000000000000000000, -1.000000000000000000 ) ) ;
#14736 = PRODUCT_CONTEXT ( 'NONE', #2750, 'mechanical' ) ;
#14737 = CARTESIAN_POINT ( 'NONE',  ( -127.7150463208621716, 87.82877071840164263, -27.51610016701188499 ) ) ;
#14738 = FACE_OUTER_BOUND ( 'NONE', #7913, .T. ) ;
#14739 = LINE ( 'NONE', #1673, #23240 ) ;
#14740 = EDGE_CURVE ( 'NONE', #13249, #5216, #9277, .T. ) ;
#14741 = ORIENTED_EDGE ( 'NONE', *, *, #1235, .T. ) ;
#14742 = CARTESIAN_POINT ( 'NONE',  ( 155.0000000000000568, -801.0618695410406644, -32.49999999999350564 ) ) ;
#14743 = EDGE_CURVE ( 'NONE', #14993, #10015, #4, .T. ) ;
#14744 = EDGE_CURVE ( 'NONE', #17675, #15759, #10054, .T. ) ;
#14745 = UNCERTAINTY_MEASURE_WITH_UNIT (LENGTH_MEASURE( 1.000000000000000082E-05 ), #20585, 'distance_accuracy_value', 'NONE');
#14746 = CARTESIAN_POINT ( 'NONE',  ( -40.00000000000000000, 100.0000000000000000, -147.2000000000005571 ) ) ;
#14747 = CARTESIAN_POINT ( 'NONE',  ( 35.00000000000000711, 0.000000000000000000, 100.0000000000000000 ) ) ;
#14748 = ORIENTED_EDGE ( 'NONE', *, *, #13790, .T. ) ;
#14749 = CARTESIAN_POINT ( 'NONE',  ( 2.500000000000002220, 1.178949249685212086, -2.042000000000002036 ) ) ;
#14750 = ORIENTED_EDGE ( 'NONE', *, *, #14060, .T. ) ;
#14751 = FACE_OUTER_BOUND ( 'NONE', #17879, .T. ) ;
#14752 = LINE ( 'NONE', #12420, #10624 ) ;
#14753 = ORIENTED_EDGE ( 'NONE', *, *, #22250, .F. ) ;
#14754 = CARTESIAN_POINT ( 'NONE',  ( -128.3589811823731281, 86.88495287852444449, -27.62619522811937856 ) ) ;
#14755 = DIRECTION ( 'NONE',  ( 4.625929269271486900E-16, 3.469446951953614978E-15, 1.000000000000000000 ) ) ;
#14756 = CARTESIAN_POINT ( 'NONE',  ( -1.636246173744678067, -1025.000000000000000, 145.0000119999999697 ) ) ;
#14757 = CARTESIAN_POINT ( 'NONE',  ( -282.1433523009093847, 268.3743436287468853, -146.2447782964893577 ) ) ;
#14758 = FACE_OUTER_BOUND ( 'NONE', #9764, .T. ) ;
#14759 = EDGE_CURVE ( 'NONE', #16847, #1157, #20122, .T. ) ;
#14760 = DIRECTION ( 'NONE',  ( -0.000000000000000000, -0.000000000000000000, 1.000000000000000000 ) ) ;
#14761 = ORIENTED_EDGE ( 'NONE', *, *, #16864, .T. ) ;
#14762 = EDGE_CURVE ( 'NONE', #6889, #9794, #5280, .T. ) ;
#14763 = DIRECTION ( 'NONE',  ( 1.000000000000000000, 0.000000000000000000, 0.000000000000000000 ) ) ;
#14764 = DIRECTION ( 'NONE',  ( -0.000000000000000000, -0.000000000000000000, 1.000000000000000000 ) ) ;
#14765 = VECTOR ( 'NONE', #7817, 1000.000000000000000 ) ;
#14767 = EDGE_LOOP ( 'NONE', ( #3185, #8107, #6362, #12989, #15615, #13012 ) ) ;
#14766 = ORIENTED_EDGE ( 'NONE', *, *, #23430, .F. ) ;
#14768 = CARTESIAN_POINT ( 'NONE',  ( 69.99999999999997158, -87.33333333333331439, 119.9999999999999716 ) ) ;
#14769 = CARTESIAN_POINT ( 'NONE',  ( -136.9911991620665788, -1072.514904345033074, -30.32927184981475577 ) ) ;
#14770 = CARTESIAN_POINT ( 'NONE',  ( 280.8708543776411943, 269.1333820183295984, -146.7350371479512887 ) ) ;
#14771 = EDGE_CURVE ( 'NONE', #4158, #6490, #6986, .T. ) ;
#14772 = ORIENTED_EDGE ( 'NONE', *, *, #22749, .T. ) ;
#14773 = ADVANCED_FACE ( 'NONE', ( #9031 ), #22357, .F. ) ;
#14774 = DIRECTION ( 'NONE',  ( 1.110223024625155594E-14, 0.000000000000000000, -1.000000000000000000 ) ) ;
#14775 = ORIENTED_EDGE ( 'NONE', *, *, #15968, .F. ) ;
#14776 = DIRECTION ( 'NONE',  ( -0.000000000000000000, -0.000000000000000000, 1.000000000000000000 ) ) ;
#14777 = EDGE_CURVE ( 'NONE', #22609, #12140, #12010, .T. ) ;
#14778 = ORIENTED_EDGE ( 'NONE', *, *, #2639, .T. ) ;
#14779 = CARTESIAN_POINT ( 'NONE',  ( 287.4000000000013415, -127.0000000000000568, 146.4928932188134638 ) ) ;
#14780 = LINE ( 'NONE', #7042, #8464 ) ;
#14781 = EDGE_CURVE ( 'NONE', #2736, #21146, #5636, .T. ) ;
#14782 = CONTEXT_DEPENDENT_SHAPE_REPRESENTATION ( #1232, #4324 ) ;
#14783 = ORIENTED_EDGE ( 'NONE', *, *, #3963, .F. ) ;
#14784 = B_SPLINE_CURVE_WITH_KNOTS ( 'NONE', 3,
 ( #23004, #8652, #21443, #8298, #6718, #4906 ),
 .UNSPECIFIED., .F., .F.,
 ( 4, 2, 4 ),
 ( 4.336808689942017736E-19, 0.0002095117440854729585, 0.0004190234881709454834 ),
 .UNSPECIFIED. ) ;
#14785 = AXIS2_PLACEMENT_3D ( 'NONE', #2019, #20034, #7116 ) ;
#14786 = APPLICATION_CONTEXT ( 'automotive_design' ) ;
#14787 = CARTESIAN_POINT ( 'NONE',  ( 124.9522429225340545, -1091.716738251577226, 32.37380477188062144 ) ) ;
#14788 = VERTEX_POINT ( 'NONE', #23741 ) ;
#14789 = CARTESIAN_POINT ( 'NONE',  ( 171.6502151485109664, 95.33502053007563859, 30.00000000000675726 ) ) ;
#14790 = CARTESIAN_POINT ( 'NONE',  ( 132.8404720734530144, 79.86494211668949106, 27.50000000000646239 ) ) ;
#14791 = CARTESIAN_POINT ( 'NONE',  ( 4.000000000000000000, -1.677850389431204459, -3.535268758346977513 ) ) ;
#14792 = CARTESIAN_POINT ( 'NONE',  ( -281.4928932188134922, 269.9999999999999432, -150.1999999999999318 ) ) ;
#14793 = CARTESIAN_POINT ( 'NONE',  ( -137.5000000000000000, -5.062647941322544249E-13, 90.00000000000000000 ) ) ;
#14794 = PLANE ( 'NONE',  #14283 ) ;
#14795 = ORIENTED_EDGE ( 'NONE', *, *, #2411, .T. ) ;
#14796 = CIRCLE ( 'NONE', #4767, 4.250000000000000000 ) ;
#14797 = SHAPE_REPRESENTATION_RELATIONSHIP ( 'NONE' , 'NONE' ,  #6236, #15670 ) ;
#14798 = ADVANCED_FACE ( 'NONE', ( #1651 ), #20346, .F. ) ;
#14799 = CARTESIAN_POINT ( 'NONE',  ( -7.500000000000000000, -2.886751345948133984, -7.198902722707428481 ) ) ;
#14800 = CARTESIAN_POINT ( 'NONE',  ( 131.5158088764654565, 82.02799531629160867, -29.83126738556711288 ) ) ;
#14801 = VECTOR ( 'NONE', #8638, 1000.000000000000000 ) ;
#14802 = EDGE_LOOP ( 'NONE', ( #3001, #5604, #9636, #2784 ) ) ;
#14803 = CARTESIAN_POINT ( 'NONE',  ( 280.8089314698394219, 269.2533442688713876, -146.6578961534456198 ) ) ;
#14804 = DIRECTION ( 'NONE',  ( -1.000000000000000000, -0.000000000000000000, -0.000000000000000000 ) ) ;
#14805 = EDGE_CURVE ( 'NONE', #15996, #14223, #16957, .T. ) ;
#14806 = CARTESIAN_POINT ( 'NONE',  ( 7.499999999999999112, 1.854554393013827296, -0.1880126015361732184 ) ) ;
#14807 = EDGE_CURVE ( 'NONE', #21417, #10987, #7197, .T. ) ;
#14808 = DIRECTION ( 'NONE',  ( 0.000000000000000000, -1.000000000000000000, 0.000000000000000000 ) ) ;
#14809 = ADVANCED_FACE ( 'NONE', ( #21927 ), #12821, .T. ) ;
#14810 = DIRECTION ( 'NONE',  ( 0.000000000000000000, 0.4999999999999992784, -0.8660254037844389297 ) ) ;
#14811 = EDGE_LOOP ( 'NONE', ( #20185, #2908, #6025, #20976 ) ) ;
#14813 = LINE ( 'NONE', #16842, #9644 ) ;
#14812 = AXIS2_PLACEMENT_3D ( 'NONE', #22301, #2253, #5782 ) ;
#14814 = ORIENTED_EDGE ( 'NONE', *, *, #9357, .F. ) ;
#14815 = DIRECTION ( 'NONE',  ( -3.495664435217746987E-15, -1.000000000000000000, 0.000000000000000000 ) ) ;
#14816 = AXIS2_PLACEMENT_3D ( 'NONE', #8426, #4797, #15236 ) ;
#14817 = CARTESIAN_POINT ( 'NONE',  ( -155.0000000000000284, -784.4690652294799520, -27.49999999999350209 ) ) ;
#14818 = LINE ( 'NONE', #5617, #11768 ) ;
#14819 = VERTEX_POINT ( 'NONE', #10745 ) ;
#14820 = CARTESIAN_POINT ( 'NONE',  ( -5.047120108843199837, 5.746297884371392328, -0.1007566405101777279 ) ) ;
#14821 = CARTESIAN_POINT ( 'NONE',  ( 123.1512869713293554, -1094.121033843497344, -28.74099766568595982 ) ) ;
#14822 = CARTESIAN_POINT ( 'NONE',  ( 145.9999999999998295, -801.0618695410399823, 27.94500000000641649 ) ) ;
#14823 = LINE ( 'NONE', #2108, #4383 ) ;
#14824 = CARTESIAN_POINT ( 'NONE',  ( 100.0000000000000000, -1400.000000000000000, -145.0000000000001705 ) ) ;
#14825 = CARTESIAN_POINT ( 'NONE',  ( -4.000000000000000000, 0.000000000000000000, 0.000000000000000000 ) ) ;
#14826 = CARTESIAN_POINT ( 'NONE',  ( -11.07878015919986581, 22.47082401081930669, 145.0000119999999697 ) ) ;
#14827 = ORIENTED_EDGE ( 'NONE', *, *, #20124, .F. ) ;
#14828 = ORIENTED_EDGE ( 'NONE', *, *, #8114, .F. ) ;
#14829 = CARTESIAN_POINT ( 'NONE',  ( -285.2000000000010118, 9.892604858775022387E-13, 146.4928932188134638 ) ) ;
#14831 = DIRECTION ( 'NONE',  ( 1.000000000000000000, 0.000000000000000000, 0.000000000000000000 ) ) ;
#14830 =( REPRESENTATION_RELATIONSHIP ('NONE','NONE', #10127, #5587 ) REPRESENTATION_RELATIONSHIP_WITH_TRANSFORMATION ( #14667 )SHAPE_REPRESENTATION_RELATIONSHIP( ) );
#14832 = ORIENTED_EDGE ( 'NONE', *, *, #4132, .T. ) ;
#14833 = CIRCLE ( 'NONE', #17511, 2.055000000000001492 ) ;
#14834 = FACE_OUTER_BOUND ( 'NONE', #19052, .T. ) ;
#14835 = CARTESIAN_POINT ( 'NONE',  ( 37.61698748598423947, 140.0355749532214702, 90.00000000000000000 ) ) ;
#14836 = DIRECTION ( 'NONE',  ( 0.000000000000000000, 0.000000000000000000, 1.000000000000000000 ) ) ;
#14837 = VERTEX_POINT ( 'NONE', #18087 ) ;
#14838 = EDGE_CURVE ( 'NONE', #3845, #13555, #21198, .T. ) ;
#14839 = CARTESIAN_POINT ( 'NONE',  ( 0.000000000000000000, 0.000000000000000000, 100.0000000000000000 ) ) ;
#14840 = EDGE_CURVE ( 'NONE', #5337, #8352, #1999, .T. ) ;
#14841 = DIRECTION ( 'NONE',  ( 0.000000000000000000, 0.000000000000000000, 1.000000000000000000 ) ) ;
#14842 = CARTESIAN_POINT ( 'NONE',  ( 0.000000000000000000, -1000.000000000000000, 90.00000000000000000 ) ) ;
#14843 = ORIENTED_EDGE ( 'NONE', *, *, #8935, .F. ) ;
#14844 = EDGE_CURVE ( 'NONE', #13544, #4142, #7924, .T. ) ;
#14845 = FACE_OUTER_BOUND ( 'NONE', #20828, .T. ) ;
#14846 = DIRECTION ( 'NONE',  ( -0.7232617928448825673, 0.6905739489807055653, 6.982962677686265922E-15 ) ) ;
#14847 = AXIS2_PLACEMENT_3D ( 'NONE', #9848, #1981, #2343 ) ;
#14848 = CARTESIAN_POINT ( 'NONE',  ( 2.500000000000002220, 0.000000000000000000, 0.000000000000000000 ) ) ;
#14849 = ORIENTED_EDGE ( 'NONE', *, *, #14124, .F. ) ;
#14850 = CARTESIAN_POINT ( 'NONE',  ( 7.907996613752301229, 3.055722423191984838, -7.792112796859423263 ) ) ;
#14851 = VECTOR ( 'NONE', #2585, 1000.000000000000114 ) ;
#14852 = PRODUCT_CONTEXT ( 'NONE', #13590, 'mechanical' ) ;
#14853 = DIRECTION ( 'NONE',  ( 0.000000000000000000, 0.000000000000000000, 1.000000000000000000 ) ) ;
#14854 = CIRCLE ( 'NONE', #13718, 45.00000000000000711 ) ;
#14855 = CARTESIAN_POINT ( 'NONE',  ( -64.99999999999995737, -52.79999999999965610, 65.00000000000017053 ) ) ;
#14856 = CARTESIAN_POINT ( 'NONE',  ( -146.0000000000000568, -494.4690652294807478, 32.05500000000641592 ) ) ;
#14857 = VECTOR ( 'NONE', #10552, 1000.000000000000227 ) ;
#14858 = CIRCLE ( 'NONE', #14480, 4.057500000000000107 ) ;
#14859 = ORIENTED_EDGE ( 'NONE', *, *, #17878, .F. ) ;
#14860 = EDGE_LOOP ( 'NONE', ( #19089, #4382, #18052, #5241 ) ) ;
#14861 = CARTESIAN_POINT ( 'NONE',  ( 155.0000000000000568, -560.0000000000000000, -60.00000000000000711 ) ) ;
#14862 = PRODUCT_DEFINITION_CONTEXT ( 'detailed design', #10639, 'design' ) ;
#14863 = FACE_OUTER_BOUND ( 'NONE', #8830, .T. ) ;
#14864 = AXIS2_PLACEMENT_3D ( 'NONE', #7596, #14989, #17144 ) ;
#14865 = DIRECTION ( 'NONE',  ( -1.000000000000000000, 1.408839003528726857E-14, 6.982962677686266711E-15 ) ) ;
#14866 = ORIENTED_EDGE ( 'NONE', *, *, #15166, .F. ) ;
#14867 = CARTESIAN_POINT ( 'NONE',  ( -79.99999999999995737, -56.79999999999918714, 250.0000000000000000 ) ) ;
#14868 = VECTOR ( 'NONE', #4704, 1000.000000000000000 ) ;
#14869 = EDGE_CURVE ( 'NONE', #11458, #6121, #16998, .T. ) ;
#14870 = VERTEX_POINT ( 'NONE', #20479 ) ;
#14871 = CARTESIAN_POINT ( 'NONE',  ( 0.000000000000000000, 0.000000000000000000, -8.499999999999998224 ) ) ;
#14872 = ORIENTED_EDGE ( 'NONE', *, *, #3797, .T. ) ;
#14873 = CARTESIAN_POINT ( 'NONE',  ( 93.00000000000000000, -149.9999999999996874, 129.9038105676659711 ) ) ;
#14874 = CARTESIAN_POINT ( 'NONE',  ( -64.99999999999995737, -52.79999999999965610, 65.00000000000017053 ) ) ;
#14875 = AXIS2_PLACEMENT_3D ( 'NONE', #4488, #6415, #21272 ) ;
#14876 = FILL_AREA_STYLE_COLOUR ( '', #21733 ) ;
#14877 = CARTESIAN_POINT ( 'NONE',  ( 284.5135885331259260, 270.4045710003932754, 145.9955614683503313 ) ) ;
#14878 = CARTESIAN_POINT ( 'NONE',  ( 124.9522429225335998, -1091.716738251577226, -27.62619522811934658 ) ) ;
#14879 = CARTESIAN_POINT ( 'NONE',  ( 2.000000000000005329, -3.464101615137751722, 0.000000000000000000 ) ) ;
#14880 = ORIENTED_EDGE ( 'NONE', *, *, #17627, .F. ) ;
#14881 = FACE_BOUND ( 'NONE', #6780, .T. ) ;
#14882 = DIRECTION ( 'NONE',  ( 1.000000000000000000, 0.000000000000000000, 0.000000000000000000 ) ) ;
#14883 =( NAMED_UNIT ( * ) PLANE_ANGLE_UNIT ( ) SI_UNIT ( $, .RADIAN. ) );
#14885 = ORIENTED_EDGE ( 'NONE', *, *, #8236, .F. ) ;
#14884 = ORIENTED_EDGE ( 'NONE', *, *, #20858, .T. ) ;
#14886 = CIRCLE ( 'NONE', #21762, 45.00000000000000711 ) ;
#14887 = DIRECTION ( 'NONE',  ( 6.123233995736766036E-17, -1.000000000000000000, 0.000000000000000000 ) ) ;
#14888 = CARTESIAN_POINT ( 'NONE',  ( -136.5850230665617460, -1073.277182683704496, -28.11073331261979291 ) ) ;
#14889 = DIRECTION ( 'NONE',  ( 0.000000000000000000, 0.000000000000000000, -1.000000000000000000 ) ) ;
#14890 = EDGE_LOOP ( 'NONE', ( #17605, #22006, #19740, #16626 ) ) ;
#14891 = CARTESIAN_POINT ( 'NONE',  ( -135.6313030678082896, -1075.027834699371169, 32.48437713430732288 ) ) ;
#14892 = ORIENTED_EDGE ( 'NONE', *, *, #20230, .F. ) ;
#14893 = AXIS2_PLACEMENT_3D ( 'NONE', #10610, #8780, #7180 ) ;
#14894 = DIRECTION ( 'NONE',  ( -1.000000000000000000, 0.000000000000000000, 0.000000000000000000 ) ) ;
#14895 = ORIENTED_EDGE ( 'NONE', *, *, #10411, .T. ) ;
#14896 = EDGE_CURVE ( 'NONE', #21860, #4834, #6241, .T. ) ;
#14897 = AXIS2_PLACEMENT_3D ( 'NONE', #19554, #10170, #17515 ) ;
#14898 = DIRECTION ( 'NONE',  ( -3.700743415417188731E-15, -1.000000000000000000, -0.000000000000000000 ) ) ;
#14899 = DIRECTION ( 'NONE',  ( -0.000000000000000000, -0.000000000000000000, 1.000000000000000000 ) ) ;
#14900 = ADVANCED_FACE ( 'NONE', ( #15310 ), #22411, .F. ) ;
#14901 = ITEM_DEFINED_TRANSFORMATION ( 'NONE', 'NONE', #12798,  #11210 ) ;
#14902 = ORIENTED_EDGE ( 'NONE', *, *, #17601, .T. ) ;
#14903 = AXIS2_PLACEMENT_3D ( 'NONE', #17674, #15893, #23226 ) ;
#14904 = CARTESIAN_POINT ( 'NONE',  ( -2.500000000000000444, 3.061616997868383634E-16, -25.03750572909317285 ) ) ;
#14905 = ORIENTED_EDGE ( 'NONE', *, *, #20929, .F. ) ;
#14906 = CARTESIAN_POINT ( 'NONE',  ( -128.0900118278593141, 87.28149574061829696, 27.50000000000646594 ) ) ;
#14907 = EDGE_CURVE ( 'NONE', #6982, #11160, #4245, .T. ) ;
#14908 = EDGE_CURVE ( 'NONE', #18021, #11437, #15190, .T. ) ;
#14909 = LINE ( 'NONE', #2077, #369 ) ;
#14910 = DIRECTION ( 'NONE',  ( 0.000000000000000000, 0.000000000000000000, -1.000000000000000000 ) ) ;
#14911 = DIRECTION ( 'NONE',  ( 0.6964005597823107463, -0.7176533009294141507, 6.982962677686266711E-15 ) ) ;
#14912 = CARTESIAN_POINT ( 'NONE',  ( -4.197393957002303999, 0.4069871074557429025, -3.503767560748926257 ) ) ;
#14913 = AXIS2_PLACEMENT_3D ( 'NONE', #1623, #9005, #20101 ) ;
#14914 = DIRECTION ( 'NONE',  ( 0.000000000000000000, 0.000000000000000000, 1.000000000000000000 ) ) ;
#14915 = ORIENTED_EDGE ( 'NONE', *, *, #11920, .T. ) ;
#14916 = ADVANCED_FACE ( 'NONE', ( #19015 ), #15080, .F. ) ;
#14917 = CARTESIAN_POINT ( 'NONE',  ( 0.000000000000000000, 0.000000000000000000, 0.000000000000000000 ) ) ;
#14918 = FACE_BOUND ( 'NONE', #13406, .T. ) ;
#14919 = CARTESIAN_POINT ( 'NONE',  ( 132.4204480437716143, 80.55959301515268578, -27.62619522811937856 ) ) ;
#14920 = VERTEX_POINT ( 'NONE', #2366 ) ;
#14921 = CARTESIAN_POINT ( 'NONE',  ( -4.197393957002303999, -7.773935952363655451E-14, -3.503767560748929810 ) ) ;
#14922 = DIRECTION ( 'NONE',  ( -0.000000000000000000, -0.000000000000000000, 1.000000000000000000 ) ) ;
#14923 = LINE ( 'NONE', #18525, #17153 ) ;
#14924 = VECTOR ( 'NONE', #12612, 1000.000000000000000 ) ;
#14925 = CARTESIAN_POINT ( 'NONE',  ( -64.99999999999998579, -52.79999999999942872, 125.0000000000001421 ) ) ;
#14926 = LINE ( 'NONE', #20211, #18867 ) ;
#14927 = DIRECTION ( 'NONE',  ( -0.000000000000000000, -0.000000000000000000, 1.000000000000000000 ) ) ;
#14928 = CONTEXT_DEPENDENT_SHAPE_REPRESENTATION ( #16647, #23368 ) ;
#14929 = ORIENTED_EDGE ( 'NONE', *, *, #21985, .F. ) ;
#14930 = DIRECTION ( 'NONE',  ( -0.000000000000000000, 1.000000000000000000, -3.469446951953613794E-15 ) ) ;
#14931 = ORIENTED_EDGE ( 'NONE', *, *, #747, .F. ) ;
#14932 = PLANE ( 'NONE',  #10666 ) ;
#14933 = FACE_BOUND ( 'NONE', #2486, .T. ) ;
#14934 = CARTESIAN_POINT ( 'NONE',  ( -175.1609685624536610, -1088.719770019218913, 27.50000000000675371 ) ) ;
#14935 = ADVANCED_FACE ( 'NONE', ( #17227 ), #13173, .F. ) ;
#14936 = ORIENTED_EDGE ( 'NONE', *, *, #12655, .T. ) ;
#14937 = CARTESIAN_POINT ( 'NONE',  ( 287.4000000000013415, -129.2000000000000455, -146.4928932188134070 ) ) ;
#14938 = CARTESIAN_POINT ( 'NONE',  ( 124.3723197571906240, -1092.501637924545548, -27.49999999999351274 ) ) ;
#14939 = EDGE_CURVE ( 'NONE', #11303, #14252, #2483, .T. ) ;
#14940 = DIRECTION ( 'NONE',  ( 1.000000000000000000, -3.495664435217746592E-15, 0.000000000000000000 ) ) ;
#14941 = DIRECTION ( 'NONE',  ( 0.000000000000000000, -3.483493295888648978E-15, -1.000000000000000000 ) ) ;
#14942 = EDGE_CURVE ( 'NONE', #4421, #19824, #20442, .T. ) ;
#14943 = DIRECTION ( 'NONE',  ( 0.000000000000000000, -1.000000000000000000, -1.177509268541832635E-16 ) ) ;
#14944 = DIRECTION ( 'NONE',  ( -0.000000000000000000, -0.000000000000000000, 1.000000000000000000 ) ) ;
#14945 = CIRCLE ( 'NONE', #12658, 2.649999999999971934 ) ;
#14946 = DIRECTION ( 'NONE',  ( 0.000000000000000000, 0.000000000000000000, -1.000000000000000000 ) ) ;
#14947 = ADVANCED_FACE ( 'NONE', ( #2235 ), #12785, .F. ) ;
#14948 = VERTEX_POINT ( 'NONE', #22644 ) ;
#14949 = FACE_BOUND ( 'NONE', #17183, .T. ) ;
#14950 = VECTOR ( 'NONE', #10040, 1000.000000000000000 ) ;
#14951 = DIRECTION ( 'NONE',  ( -1.000000000000000000, 1.408839003528726857E-14, 6.982962677686266711E-15 ) ) ;
#14952 = EDGE_CURVE ( 'NONE', #4961, #12471, #18147, .T. ) ;
#14953 = EDGE_LOOP ( 'NONE', ( #13633, #20835 ) ) ;
#14954 = CARTESIAN_POINT ( 'NONE',  ( 5.878908934339781567, 8.175523358512194250, 200.0000120000000265 ) ) ;
#14955 = CARTESIAN_POINT ( 'NONE',  ( 70.00000000000000000, -87.33333333333332860, 3.000000000000001332 ) ) ;
#14956 = DIRECTION ( 'NONE',  ( 0.000000000000000000, 0.000000000000000000, 1.000000000000000000 ) ) ;
#14957 = ORIENTED_EDGE ( 'NONE', *, *, #3434, .T. ) ;
#14958 = CARTESIAN_POINT ( 'NONE',  ( 0.000000000000000000, 1.178949249685212974, -2.042000000000001148 ) ) ;
#14959 = DIRECTION ( 'NONE',  ( -0.000000000000000000, -0.000000000000000000, -1.000000000000000000 ) ) ;
#14960 = CIRCLE ( 'NONE', #13826, 7.499999999999998224 ) ;
#14961 = CARTESIAN_POINT ( 'NONE',  ( 7.996668423981803109, -6.145467199749149678, 200.0000120000000834 ) ) ;
#14962 = ORIENTED_EDGE ( 'NONE', *, *, #23189, .F. ) ;
#14963 = CARTESIAN_POINT ( 'NONE',  ( 0.000000000000000000, -1000.000000000000000, 138.9999999999999716 ) ) ;
#14964 = FACE_OUTER_BOUND ( 'NONE', #211, .T. ) ;
#14965 = CIRCLE ( 'NONE', #11512, 7.500000000000000888 ) ;
#14966 = CARTESIAN_POINT ( 'NONE',  ( 45.00000000000002132, -52.79999999999936477, 140.0000000000001990 ) ) ;
#14967 = VECTOR ( 'NONE', #18214, 1000.000000000000000 ) ;
#14968 = ORIENTED_EDGE ( 'NONE', *, *, #4517, .T. ) ;
#14969 = CARTESIAN_POINT ( 'NONE',  ( 283.1956429438695295, 271.9582675804705332, -145.6220388411722126 ) ) ;
#14970 = VECTOR ( 'NONE', #21761, 1000.000000000000000 ) ;
#14971 = APPLICATION_PROTOCOL_DEFINITION ( 'draft international standard', 'automotive_design', 1998, #16775 ) ;
#14972 = DIRECTION ( 'NONE',  ( -8.144298233840332611E-17, 0.000000000000000000, -1.000000000000000000 ) ) ;
#14973 = CARTESIAN_POINT ( 'NONE',  ( -90.00000000000000000, -74.99999999999998579, 3.000000000000000000 ) ) ;
#14974 = DIRECTION ( 'NONE',  ( -0.9423651898111408132, -0.3345860861306287348, 6.982962677686266711E-15 ) ) ;
#14975 = VERTEX_POINT ( 'NONE', #22777 ) ;
#14977 = EDGE_LOOP ( 'NONE', ( #15014, #15130, #20793, #3233 ) ) ;
#14976 = EDGE_CURVE ( 'NONE', #13294, #3415, #4307, .T. ) ;
#14978 = EDGE_CURVE ( 'NONE', #17788, #14948, #782, .T. ) ;
#14979 = CARTESIAN_POINT ( 'NONE',  ( -8.055391459054607850, -23.72315261474502890, 145.0000119999999981 ) ) ;
#14980 = CARTESIAN_POINT ( 'NONE',  ( 50.00000000000000000, -137.1994082814340743, -2.400000000000046096 ) ) ;
#14981 = EDGE_CURVE ( 'NONE', #13599, #14601, #22759, .T. ) ;
#14982 = AXIS2_PLACEMENT_3D ( 'NONE', #5757, #20586, #4418 ) ;
#14983 = AXIS2_PLACEMENT_3D ( 'NONE', #554, #11815, #19005 ) ;
#14984 = ORIENTED_EDGE ( 'NONE', *, *, #12478, .F. ) ;
#14985 = DIRECTION ( 'NONE',  ( 0.000000000000000000, -1.000000000000000000, 0.000000000000000000 ) ) ;
#14986 = AXIS2_PLACEMENT_3D ( 'NONE', #4672, #1390, #2949 ) ;
#14987 = CARTESIAN_POINT ( 'NONE',  ( 117.3074641843663386, 85.22886158241004750, 90.00000000000000000 ) ) ;
#14988 = ORIENTED_EDGE ( 'NONE', *, *, #22168, .T. ) ;
#14989 = DIRECTION ( 'NONE',  ( -1.000000000000000000, 3.495664435217746987E-15, 0.000000000000000000 ) ) ;
#14990 = VERTEX_POINT ( 'NONE', #22520 ) ;
#14991 = DIRECTION ( 'NONE',  ( 0.000000000000000000, 0.000000000000000000, 1.000000000000000000 ) ) ;
#14992 = LINE ( 'NONE', #11271, #22919 ) ;
#14993 = VERTEX_POINT ( 'NONE', #13399 ) ;
#14994 = CARTESIAN_POINT ( 'NONE',  ( -285.2000000000012960, -74.99999999999899103, -90.00000000000000000 ) ) ;
#14995 = DIRECTION ( 'NONE',  ( 0.000000000000000000, 0.000000000000000000, -1.000000000000000000 ) ) ;
#14996 = CIRCLE ( 'NONE', #21522, 8.000000000000000000 ) ;
#14997 = CARTESIAN_POINT ( 'NONE',  ( 22.47082401081929603, -1011.078780159200051, 145.0000119999999697 ) ) ;
#14998 = AXIS2_PLACEMENT_3D ( 'NONE', #16947, #15152, #17068 ) ;
#14999 = FACE_OUTER_BOUND ( 'NONE', #11495, .T. ) ;
#15000 = DIRECTION ( 'NONE',  ( 1.000000000000000000, 0.000000000000000000, 0.000000000000000000 ) ) ;
#15001 = CIRCLE ( 'NONE', #20381, 2.649999999999985700 ) ;
#15002 = CARTESIAN_POINT ( 'NONE',  ( -31.74999999999995737, 0.000000000000000000, 2.500000000000000444 ) ) ;
#15003 = EDGE_LOOP ( 'NONE', ( #19303, #16860, #14144, #969 ) ) ;
#15004 = CARTESIAN_POINT ( 'NONE',  ( 5.000000000000002665, 0.000000000000000000, -2.700000000000000622 ) ) ;
#15005 = DIRECTION ( 'NONE',  ( -1.350636282998972974E-14, 0.000000000000000000, -1.000000000000000000 ) ) ;
#15006 = AXIS2_PLACEMENT_3D ( 'NONE', #2957, #8196, #21225 ) ;
#15008 = EDGE_LOOP ( 'NONE', ( #10888, #1424, #2885, #11655 ) ) ;
#15007 = ORIENTED_EDGE ( 'NONE', *, *, #1941, .F. ) ;
#15009 = LINE ( 'NONE', #18598, #5791 ) ;
#15010 = DIRECTION ( 'NONE',  ( 0.000000000000000000, -1.177509268541832635E-16, 1.000000000000000000 ) ) ;
#15011 = EDGE_LOOP ( 'NONE', ( #9266, #10827, #13347 ) ) ;
#15012 = AXIS2_PLACEMENT_3D ( 'NONE', #14364, #20112, #12676 ) ;
#15013 = CARTESIAN_POINT ( 'NONE',  ( 10.40000000000000036, 0.000000000000000000, 0.000000000000000000 ) ) ;
#15014 = ORIENTED_EDGE ( 'NONE', *, *, #62, .F. ) ;
#15015 = CONICAL_SURFACE ( 'NONE', #12021, 2.055000000000001492, 0.7853981633974633780 ) ;
#15016 = CARTESIAN_POINT ( 'NONE',  ( 285.1663407402830899, 268.4822561791008866, -146.3681929792553547 ) ) ;
#15017 = AXIS2_PLACEMENT_3D ( 'NONE', #10325, #15994, #17669 ) ;
#15018 = CIRCLE ( 'NONE', #18477, 5.000000000000000888 ) ;
#15019 = ORIENTED_EDGE ( 'NONE', *, *, #10602, .F. ) ;
#15020 = DIRECTION ( 'NONE',  ( 0.000000000000000000, -1.000000000000000000, 0.000000000000000000 ) ) ;
#15021 = DIRECTION ( 'NONE',  ( 1.000000000000000000, 0.000000000000000000, 0.000000000000000000 ) ) ;
#15022 = AXIS2_PLACEMENT_3D ( 'NONE', #1471, #21653, #21520 ) ;
#15023 = EDGE_LOOP ( 'NONE', ( #9936, #7261 ) ) ;
#15024 = CARTESIAN_POINT ( 'NONE',  ( -282.2000000000013529, -89.99999999999897682, 21.68333333333335844 ) ) ;
#15025 = ORIENTED_EDGE ( 'NONE', *, *, #11292, .T. ) ;
#15026 = DIRECTION ( 'NONE',  ( -1.000000000000000000, -3.736327486719275871E-16, -0.000000000000000000 ) ) ;
#15027 = FILL_AREA_STYLE ('',( #18729 ) ) ;
#15028 = EDGE_CURVE ( 'NONE', #5008, #590, #5991, .T. ) ;
#15029 = FACE_OUTER_BOUND ( 'NONE', #7684, .T. ) ;
#15030 = CIRCLE ( 'NONE', #22325, 7.500000000000001776 ) ;
#15031 = VECTOR ( 'NONE', #14542, 1000.000000000000000 ) ;
#15032 = DIRECTION ( 'NONE',  ( 0.000000000000000000, -1.177509268541832635E-16, 1.000000000000000000 ) ) ;
#15033 = EDGE_LOOP ( 'NONE', ( #22794, #8219, #3149, #19139 ) ) ;
#15035 = AXIS2_PLACEMENT_3D ( 'NONE', #18271, #167, #19854 ) ;
#15034 = COLOUR_RGB ( '',1.000000000000000000, 0.9490196078431372140, 0.9098039215686274384 ) ;
#15036 = CARTESIAN_POINT ( 'NONE',  ( -280.4976310729378497, 269.6958543268121957, -146.0927021017107279 ) ) ;
#15037 = AXIS2_PLACEMENT_3D ( 'NONE', #16279, #23622, #3327 ) ;
#15038 = VECTOR ( 'NONE', #19605, 999.9999999999998863 ) ;
#15039 = VECTOR ( 'NONE', #4509, 1000.000000000000000 ) ;
#15040 = CIRCLE ( 'NONE', #6544, 10.39117206796836079 ) ;
#15041 = AXIS2_PLACEMENT_3D ( 'NONE', #1414, #3568, #3338 ) ;
#15042 = ORIENTED_EDGE ( 'NONE', *, *, #19897, .F. ) ;
#15043 = ADVANCED_FACE ( 'NONE', ( #18907 ), #2186, .F. ) ;
#15044 = CARTESIAN_POINT ( 'NONE',  ( 0.000000000000000000, -1000.000000000000000, 0.000000000000000000 ) ) ;
#15045 = DIRECTION ( 'NONE',  ( 0.000000000000000000, 1.177509268541832635E-16, -1.000000000000000000 ) ) ;
#15046 = CARTESIAN_POINT ( 'NONE',  ( 121.5574576620388143, 79.04925354955381067, -90.00000000000000000 ) ) ;
#15047 = EDGE_CURVE ( 'NONE', #12879, #8456, #23125, .T. ) ;
#15048 = CARTESIAN_POINT ( 'NONE',  ( 283.2140793454687469, 271.9822575857424454, 145.6220388411722979 ) ) ;
#15049 = CARTESIAN_POINT ( 'NONE',  ( -280.0000000000000568, 273.0299999999999159, -144.9999999999999716 ) ) ;
#15050 = EDGE_CURVE ( 'NONE', #12140, #22609, #21217, .T. ) ;
#15052 = VECTOR ( 'NONE', #4822, 1000.000000000000000 ) ;
#15051 = PRESENTATION_LAYER_ASSIGNMENT (  '', '', ( #6554 ) ) ;
#15053 = DIRECTION ( 'NONE',  ( 3.469446951953614682E-16, -1.000000000000000000, 3.483493295888648978E-15 ) ) ;
#15054 = FACE_OUTER_BOUND ( 'NONE', #21850, .T. ) ;
#15055 = VECTOR ( 'NONE', #16099, 1000.000000000000000 ) ;
#15056 = CONTEXT_DEPENDENT_SHAPE_REPRESENTATION ( #16504, #19705 ) ;
#15057 = ORIENTED_EDGE ( 'NONE', *, *, #11732, .T. ) ;
#15058 = AXIS2_PLACEMENT_3D ( 'NONE', #128, #3379, #18135 ) ;
#15059 = VECTOR ( 'NONE', #13045, 1000.000000000000000 ) ;
#15060 = DIRECTION ( 'NONE',  ( -0.5000000000000051070, 1.060575238724903217E-16, -0.8660254037844355990 ) ) ;
#15061 = ORIENTED_EDGE ( 'NONE', *, *, #6196, .F. ) ;
#15062 = DIRECTION ( 'NONE',  ( 0.000000000000000000, -1.110223024625156540E-16, 1.000000000000000000 ) ) ;
#15063 = SURFACE_STYLE_USAGE ( .BOTH. , #3913 ) ;
#15064 = CARTESIAN_POINT ( 'NONE',  ( 2.500000000000002220, -1.178949249685215417, 2.042000000000002036 ) ) ;
#15065 = ORIENTED_EDGE ( 'NONE', *, *, #22720, .F. ) ;
#15066 = FACE_OUTER_BOUND ( 'NONE', #4908, .T. ) ;
#15067 = VECTOR ( 'NONE', #10131, 1000.000000000000000 ) ;
#15068 = CARTESIAN_POINT ( 'NONE',  ( 123.9854850298561786, -1093.019475613610211, -27.62591505085370258 ) ) ;
#15069 = DIRECTION ( 'NONE',  ( -0.000000000000000000, -0.000000000000000000, 1.000000000000000000 ) ) ;
#15070 = LINE ( 'NONE', #5863, #20573 ) ;
#15071 = CARTESIAN_POINT ( 'NONE',  ( 146.0000000000002274, -801.0618695410406644, -29.99999999999356604 ) ) ;
#15072 = LINE ( 'NONE', #200, #21552 ) ;
#15073 = CARTESIAN_POINT ( 'NONE',  ( -7.499999999999650058, -0.7583608255766450812, -7.446489218764574147 ) ) ;
#15074 = EDGE_LOOP ( 'NONE', ( #23796, #1582, #12711, #18101 ) ) ;
#15075 = PRODUCT_DEFINITION_FORMATION_WITH_SPECIFIED_SOURCE ( 'ANY', '', #6496, .NOT_KNOWN. ) ;
#15076 = CARTESIAN_POINT ( 'NONE',  ( 281.4928932188133217, 267.7999999999999545, 147.1999999999999886 ) ) ;
#15077 = DIRECTION ( 'NONE',  ( -0.000000000000000000, -0.000000000000000000, 1.000000000000000000 ) ) ;
#15078 = AXIS2_PLACEMENT_3D ( 'NONE', #4423, #13653, #15313 ) ;
#15079 = ORIENTED_EDGE ( 'NONE', *, *, #8123, .T. ) ;
#15080 = CONICAL_SURFACE ( 'NONE', #8909, 2.055000000000001492, 0.7853981633974633780 ) ;
#15081 = ORIENTED_EDGE ( 'NONE', *, *, #3872, .F. ) ;
#15082 = DIRECTION ( 'NONE',  ( 1.000000000000000000, 0.000000000000000000, 0.000000000000000000 ) ) ;
#15083 = DIRECTION ( 'NONE',  ( 8.144298233840332611E-17, 3.483493295888648978E-15, 1.000000000000000000 ) ) ;
#15084 = EDGE_CURVE ( 'NONE', #1956, #10702, #5036, .T. ) ;
#15085 = DIRECTION ( 'NONE',  ( -0.5000000000000051070, 1.060575238724903217E-16, -0.8660254037844355990 ) ) ;
#15086 = EDGE_CURVE ( 'NONE', #10091, #5513, #4536, .T. ) ;
#15087 = VERTEX_POINT ( 'NONE', #11949 ) ;
#15088 = CARTESIAN_POINT ( 'NONE',  ( 70.00000000000000000, -112.6666666666666714, 124.9999999999999858 ) ) ;
#15089 = DIRECTION ( 'NONE',  ( 0.9289202219288174023, 0.3702799228849934510, 6.982962677686266711E-15 ) ) ;
#15090 = ADVANCED_FACE ( 'NONE', ( #19261 ), #10228, .T. ) ;
#15091 = CARTESIAN_POINT ( 'NONE',  ( 232.0000000000000284, 3.319562792410127342E-14, -56.99999999999973710 ) ) ;
#15092 = EDGE_LOOP ( 'NONE', ( #15990, #16924, #19388, #8749 ) ) ;
#15093 = CARTESIAN_POINT ( 'NONE',  ( 280.4973317504630472, 272.3135885331258805, 147.6045710003933777 ) ) ;
#15094 = CARTESIAN_POINT ( 'NONE',  ( -69.99999999999997158, -112.6666666666667140, 3.000000000000001332 ) ) ;
#15095 = FACE_OUTER_BOUND ( 'NONE', #8928, .T. ) ;
#15096 = EDGE_CURVE ( 'NONE', #15482, #22916, #18, .T. ) ;
#15097 = DIRECTION ( 'NONE',  ( 0.000000000000000000, -0.4999999999999991118, 0.8660254037844391517 ) ) ;
#15098 = EDGE_LOOP ( 'NONE', ( #4614, #8198 ) ) ;
#15099 = FACE_OUTER_BOUND ( 'NONE', #15011, .T. ) ;
#15100 = PRODUCT_CONTEXT ( 'NONE', #15572, 'mechanical' ) ;
#15101 = DIRECTION ( 'NONE',  ( 0.000000000000000000, -1.000000000000000000, 0.000000000000000000 ) ) ;
#15102 = CARTESIAN_POINT ( 'NONE',  ( 100.0000000000000000, -1420.000000000000000, 144.9999999999998295 ) ) ;
#15103 = CYLINDRICAL_SURFACE ( 'NONE', #17081, 2.500000000000002220 ) ;
#15104 = ORIENTED_EDGE ( 'NONE', *, *, #14976, .T. ) ;
#15105 = ORIENTED_EDGE ( 'NONE', *, *, #18716, .T. ) ;
#15106 = LINE ( 'NONE', #2511, #20707 ) ;
#15107 = FACE_OUTER_BOUND ( 'NONE', #8660, .T. ) ;
#15108 = EDGE_CURVE ( 'NONE', #6672, #10540, #18129, .T. ) ;
#15109 = UNCERTAINTY_MEASURE_WITH_UNIT (LENGTH_MEASURE( 1.000000000000000082E-05 ), #10843, 'distance_accuracy_value', 'NONE');
#15110 =( REPRESENTATION_RELATIONSHIP ('NONE','NONE', #10127, #18083 ) REPRESENTATION_RELATIONSHIP_WITH_TRANSFORMATION ( #13261 )SHAPE_REPRESENTATION_RELATIONSHIP( ) );
#15111 = ORIENTED_EDGE ( 'NONE', *, *, #11176, .T. ) ;
#15112 = CARTESIAN_POINT ( 'NONE',  ( -288.2000000000008981, 35.00000000000100897, 102.3500000000000227 ) ) ;
#15113 = CARTESIAN_POINT ( 'NONE',  ( -146.0000000000001421, -496.5240652294807546, 30.00000000000641620 ) ) ;
#15114 = VERTEX_POINT ( 'NONE', #17462 ) ;
#15115 = DIRECTION ( 'NONE',  ( 0.000000000000000000, 0.000000000000000000, 1.000000000000000000 ) ) ;
#15116 = ORIENTED_EDGE ( 'NONE', *, *, #4332, .T. ) ;
#15117 = EDGE_CURVE ( 'NONE', #14121, #21414, #8289, .T. ) ;
#15118 = CARTESIAN_POINT ( 'NONE',  ( 99.99999999999994316, 4.509448885211231533E-13, 150.2000000000009550 ) ) ;
#15119 = EDGE_CURVE ( 'NONE', #15297, #6312, #6465, .T. ) ;
#15120 = CARTESIAN_POINT ( 'NONE',  ( 0.000000000000000000, 2.342598717236902939, -4.057500000000001883 ) ) ;
#15121 = ORIENTED_EDGE ( 'NONE', *, *, #13600, .T. ) ;
#15122 = ORIENTED_EDGE ( 'NONE', *, *, #21503, .F. ) ;
#15123 = DIRECTION ( 'NONE',  ( 0.000000000000000000, -3.469446951953613794E-15, -1.000000000000000000 ) ) ;
#15124 = CARTESIAN_POINT ( 'NONE',  ( -280.5908103165960483, 272.0295083325148653, -148.0299054689546665 ) ) ;
#15125 = CARTESIAN_POINT ( 'NONE',  ( -24.99995073929423484, -1001.642023388033635, -145.0000000000001137 ) ) ;
#15126 = DIRECTION ( 'NONE',  ( 1.000000000000000000, -3.495664435217746987E-15, -0.000000000000000000 ) ) ;
#15127 = LINE ( 'NONE', #17044, #6919 ) ;
#15128 = LINE ( 'NONE', #20641, #4716 ) ;
#15129 = CARTESIAN_POINT ( 'NONE',  ( 3.355112389629172576, -2.681727112203168950, -0.2256878752776777242 ) ) ;
#15130 = ORIENTED_EDGE ( 'NONE', *, *, #4795, .T. ) ;
#15131 = DIRECTION ( 'NONE',  ( -1.000000000000000000, -0.000000000000000000, -0.000000000000000000 ) ) ;
#15132 = CARTESIAN_POINT ( 'NONE',  ( -4.211140560182196957, -2.431303136016552013, -3.745885042887436178 ) ) ;
#15134 = ORIENTED_EDGE ( 'NONE', *, *, #9299, .F. ) ;
#15133 = ORIENTED_EDGE ( 'NONE', *, *, #22088, .F. ) ;
#15135 = CARTESIAN_POINT ( 'NONE',  ( -69.99999999999997158, -112.6666666666667140, 148.0000000000000000 ) ) ;
#15136 = CARTESIAN_POINT ( 'NONE',  ( 281.2440776823445390, 269.1610889986682764, -150.0646579186751808 ) ) ;
#15137 = ORIENTED_EDGE ( 'NONE', *, *, #14838, .F. ) ;
#15138 = CARTESIAN_POINT ( 'NONE',  ( -146.0000000000005116, -784.4690652294799520, -29.99999999999356604 ) ) ;
#15139 = ORIENTED_EDGE ( 'NONE', *, *, #1940, .F. ) ;
#15140 = LINE ( 'NONE', #22228, #23432 ) ;
#15141 = ORIENTED_EDGE ( 'NONE', *, *, #20131, .T. ) ;
#15142 = ADVANCED_FACE ( 'NONE', ( #10483 ), #906, .T. ) ;
#15143 = DIRECTION ( 'NONE',  ( 1.000000000000000000, 0.000000000000000000, 0.000000000000000000 ) ) ;
#15144 = ITEM_DEFINED_TRANSFORMATION ( 'NONE', 'NONE', #5801,  #11210 ) ;
#15145 = VERTEX_POINT ( 'NONE', #8642 ) ;
#15146 = ADVANCED_FACE ( 'NONE', ( #13995 ), #21320, .T. ) ;
#15147 = CARTESIAN_POINT ( 'NONE',  ( -25.00000000000001776, 45.00100000000062295, 124.9999999999998579 ) ) ;
#15148 = EDGE_LOOP ( 'NONE', ( #21348, #23689, #7401, #5333 ) ) ;
#15149 = CARTESIAN_POINT ( 'NONE',  ( -128.5309343563513380, 86.63037569149894068, 27.75096515221181193 ) ) ;
#15150 = PLANE ( 'NONE',  #16948 ) ;
#15151 = AXIS2_PLACEMENT_3D ( 'NONE', #22788, #22531, #917 ) ;
#15152 = DIRECTION ( 'NONE',  ( 0.000000000000000000, -1.000000000000000000, 0.000000000000000000 ) ) ;
#15153 = DIRECTION ( 'NONE',  ( 1.000000000000000000, 0.000000000000000000, 0.000000000000000000 ) ) ;
#15154 = EDGE_LOOP ( 'NONE', ( #12240, #14163, #10450, #4494 ) ) ;
#15155 = CARTESIAN_POINT ( 'NONE',  ( -281.3684665479255500, 268.0880230824753312, -147.1999999999999318 ) ) ;
#15156 = ORIENTED_EDGE ( 'NONE', *, *, #10372, .T. ) ;
#15157 = CARTESIAN_POINT ( 'NONE',  ( 0.000000000000000000, -301.0618695410403234, 0.000000000000000000 ) ) ;
#15158 = PLANE ( 'NONE',  #20421 ) ;
#15159 = DIRECTION ( 'NONE',  ( 0.000000000000000000, 0.000000000000000000, 1.000000000000000000 ) ) ;
#15160 = DIRECTION ( 'NONE',  ( 0.000000000000000000, 0.000000000000000000, 1.000000000000000000 ) ) ;
#15161 = CARTESIAN_POINT ( 'NONE',  ( 0.000000000000000000, 0.000000000000000000, -4.000000000000000000 ) ) ;
#15162 = VERTEX_POINT ( 'NONE', #19490 ) ;
#15163 = ADVANCED_FACE ( 'NONE', ( #2943 ), #17690, .F. ) ;
#15164 = AXIS2_PLACEMENT_3D ( 'NONE', #11734, #11480, #13670 ) ;
#15165 = CARTESIAN_POINT ( 'NONE',  ( -8.964803508279640454, 4.586180457551869871, 200.0000119999999981 ) ) ;
#15166 = EDGE_CURVE ( 'NONE', #2346, #16143, #19403, .T. ) ;
#15167 = DIRECTION ( 'NONE',  ( 0.9510565162951534202, 0.3090169943749478398, 0.000000000000000000 ) ) ;
#15168 = CARTESIAN_POINT ( 'NONE',  ( -100.0000000000000000, -1400.000000000000000, -145.0000000000001705 ) ) ;
#15169 = CONTEXT_DEPENDENT_SHAPE_REPRESENTATION ( #13901, #7003 ) ;
#15170 = ORIENTED_EDGE ( 'NONE', *, *, #21893, .F. ) ;
#15171 = CARTESIAN_POINT ( 'NONE',  ( 121.5574576620388143, 79.04925354955381067, 90.00000000000000000 ) ) ;
#15172 = ORIENTED_EDGE ( 'NONE', *, *, #9923, .T. ) ;
#15173 = ADVANCED_FACE ( 'NONE', ( #9247 ), #10846, .T. ) ;
#15174 = DIRECTION ( 'NONE',  ( 0.000000000000000000, -1.000000000000000000, 0.000000000000000000 ) ) ;
#15175 = FACE_OUTER_BOUND ( 'NONE', #6243, .T. ) ;
#15176 = ORIENTED_EDGE ( 'NONE', *, *, #13545, .T. ) ;
#15177 = CARTESIAN_POINT ( 'NONE',  ( -20.63749999999999929, 0.000000000000000000, 0.000000000000000000 ) ) ;
#15178 = VERTEX_POINT ( 'NONE', #7168 ) ;
#15179 = DIRECTION ( 'NONE',  ( -0.000000000000000000, -0.000000000000000000, 1.000000000000000000 ) ) ;
#15180 = DIRECTION ( 'NONE',  ( 0.000000000000000000, 0.000000000000000000, 1.000000000000000000 ) ) ;
#15181 = DIRECTION ( 'NONE',  ( 0.000000000000000000, 0.000000000000000000, 1.000000000000000000 ) ) ;
#15182 = DIRECTION ( 'NONE',  ( -1.000000000000000000, -2.775557561562891351E-17, 0.000000000000000000 ) ) ;
#15183 = FACE_OUTER_BOUND ( 'NONE', #15479, .T. ) ;
#15184 = ADVANCED_FACE ( 'NONE', ( #21676 ), #21560, .T. ) ;
#15185 = DIRECTION ( 'NONE',  ( 0.000000000000000000, 0.000000000000000000, 1.000000000000000000 ) ) ;
#15186 = CARTESIAN_POINT ( 'NONE',  ( -7.499999999999999112, -4.652405105468739421, -7.929127756970856034 ) ) ;
#15187 = VECTOR ( 'NONE', #17816, 1000.000000000000000 ) ;
#15188 = ORIENTED_EDGE ( 'NONE', *, *, #20078, .T. ) ;
#15189 = DIRECTION ( 'NONE',  ( 0.000000000000000000, 0.000000000000000000, 1.000000000000000000 ) ) ;
#15190 = LINE ( 'NONE', #4173, #3861 ) ;
#15191 = ORIENTED_EDGE ( 'NONE', *, *, #21253, .T. ) ;
#15192 = ORIENTED_EDGE ( 'NONE', *, *, #12899, .T. ) ;
#15193 = PLANE ( 'NONE',  #13947 ) ;
#15194 = CARTESIAN_POINT ( 'NONE',  ( 0.000000000000000000, 0.000000000000000000, 90.00000000000000000 ) ) ;
#15195 = LINE ( 'NONE', #5769, #17536 ) ;
#15196 = AXIS2_PLACEMENT_3D ( 'NONE', #11873, #19536, #12005 ) ;
#15197 = MECHANICAL_DESIGN_GEOMETRIC_PRESENTATION_REPRESENTATION (  '', ( #7853 ), #17490 ) ;
#15198 = ORIENTED_EDGE ( 'NONE', *, *, #18957, .T. ) ;
#15199 = CARTESIAN_POINT ( 'NONE',  ( 107.6499999999999631, -19.99999999999998934, 3.000000000000000000 ) ) ;
#15200 = DIRECTION ( 'NONE',  ( -0.000000000000000000, -1.177509268541832635E-16, 1.000000000000000000 ) ) ;
#15201 = CARTESIAN_POINT ( 'NONE',  ( 2.059999999999998721, 0.000000000000000000, -0.3080913168122742518 ) ) ;
#15202 = ORIENTED_EDGE ( 'NONE', *, *, #313, .F. ) ;
#15203 = EDGE_CURVE ( 'NONE', #16635, #23462, #5308, .T. ) ;
#15204 = CARTESIAN_POINT ( 'NONE',  ( 4.204015924366189871, -1.626724848190933548, -3.610627190413393084 ) ) ;
#15205 = CARTESIAN_POINT ( 'NONE',  ( -31.74999999999995737, 9.797174393178825657E-16, -8.000000000000000000 ) ) ;
#15206 = ADVANCED_FACE ( 'NONE', ( #5252 ), #520, .F. ) ;
#15207 = CARTESIAN_POINT ( 'NONE',  ( -1.500000000000000000, 0.000000000000000000, 150.0000000000000284 ) ) ;
#15208 = ORIENTED_EDGE ( 'NONE', *, *, #22126, .T. ) ;
#15209 = CARTESIAN_POINT ( 'NONE',  ( 282.1132285165672329, 268.3679143846943020, -146.2440776823444537 ) ) ;
#15210 = FACE_BOUND ( 'NONE', #19659, .T. ) ;
#15211 = EDGE_CURVE ( 'NONE', #15625, #7880, #5412, .T. ) ;
#15212 = CARTESIAN_POINT ( 'NONE',  ( -7.298354728638373423, 4.926141412641537265, -7.913704048100170141 ) ) ;
#15213 = DIRECTION ( 'NONE',  ( 1.000000000000000000, 0.000000000000000000, 0.000000000000000000 ) ) ;
#15214 = AXIS2_PLACEMENT_3D ( 'NONE', #7181, #1281, #8659 ) ;
#15215 = ADVANCED_FACE ( 'NONE', ( #18174 ), #20098, .F. ) ;
#15216 = ORIENTED_EDGE ( 'NONE', *, *, #7996, .F. ) ;
#15217 = AXIS2_PLACEMENT_3D ( 'NONE', #5916, #2160, #20638 ) ;
#15218 = VERTEX_POINT ( 'NONE', #5374 ) ;
#15219 = CARTESIAN_POINT ( 'NONE',  ( -34.75000000000005684, 100.0000000000000000, -150.2000000000005571 ) ) ;
#15220 = DIRECTION ( 'NONE',  ( -1.000000000000000000, 1.408839003528726857E-14, 6.982962677686266711E-15 ) ) ;
#15221 = EDGE_CURVE ( 'NONE', #8352, #22022, #10953, .T. ) ;
#15222 = ORIENTED_EDGE ( 'NONE', *, *, #21071, .T. ) ;
#15223 = FACE_OUTER_BOUND ( 'NONE', #13481, .T. ) ;
#15224 = CARTESIAN_POINT ( 'NONE',  ( -127.7157292285634753, 87.82777678213082595, 27.51597717546056998 ) ) ;
#15225 = EDGE_LOOP ( 'NONE', ( #9082, #17448, #18752, #16708 ) ) ;
#15226 = DIRECTION ( 'NONE',  ( -0.000000000000000000, 0.8660254037844393737, 0.4999999999999988343 ) ) ;
#15227 =( GEOMETRIC_REPRESENTATION_CONTEXT ( 3 ) GLOBAL_UNCERTAINTY_ASSIGNED_CONTEXT ( ( #17255 ) ) GLOBAL_UNIT_ASSIGNED_CONTEXT ( ( #7946, #18790, #4192 ) ) REPRESENTATION_CONTEXT ( 'NONE', 'WORKASPACE' ) );
#15228 = EDGE_LOOP ( 'NONE', ( #3640, #10726 ) ) ;
#15229 = AXIS2_PLACEMENT_3D ( 'NONE', #1615, #7162, #10946 ) ;
#15230 = CARTESIAN_POINT ( 'NONE',  ( 0.000000000000000000, 0.000000000000000000, -90.00000000000000000 ) ) ;
#15231 = CARTESIAN_POINT ( 'NONE',  ( 0.000000000000000000, 0.000000000000000000, 100.0000000000000000 ) ) ;
#15232 = ORIENTED_EDGE ( 'NONE', *, *, #5004, .T. ) ;
#15233 = VERTEX_POINT ( 'NONE', #16472 ) ;
#15234 = CARTESIAN_POINT ( 'NONE',  ( 0.000000000000000000, 0.000000000000000000, -138.9999999999999716 ) ) ;
#15235 = EDGE_CURVE ( 'NONE', #11911, #5651, #399, .T. ) ;
#15236 = DIRECTION ( 'NONE',  ( -4.625929269271472109E-16, 0.000000000000000000, 1.000000000000000000 ) ) ;
#15237 = ADVANCED_FACE ( 'NONE', ( #13011 ), #11200, .T. ) ;
#15238 = CARTESIAN_POINT ( 'NONE',  ( 10.39117206796836079, 1.272551561242683567E-15, -8.499999999999998224 ) ) ;
#15239 = CARTESIAN_POINT ( 'NONE',  ( 2.500000000000000000, 1.768423874527825124, 1.020999999999998797 ) ) ;
#15240 = CARTESIAN_POINT ( 'NONE',  ( -4.000000000000000000, -2.309401076758512694, -5.000000000000000000 ) ) ;
#15241 = ADVANCED_FACE ( 'NONE', ( #536 ), #649, .T. ) ;
#15242 = FACE_OUTER_BOUND ( 'NONE', #22310, .T. ) ;
#15243 = ORIENTED_EDGE ( 'NONE', *, *, #1188, .F. ) ;
#15244 = EDGE_CURVE ( 'NONE', #17523, #6254, #12404, .T. ) ;
#15245 = CARTESIAN_POINT ( 'NONE',  ( 0.000000000000000000, 0.000000000000000000, 0.000000000000000000 ) ) ;
#15246 = DIRECTION ( 'NONE',  ( 0.000000000000000000, 0.000000000000000000, -1.000000000000000000 ) ) ;
#15247 = VERTEX_POINT ( 'NONE', #2335 ) ;
#15248 = EDGE_CURVE ( 'NONE', #4937, #4516, #6560, .T. ) ;
#15249 = CARTESIAN_POINT ( 'NONE',  ( -136.3245111336061086, -1073.760768802671691, -32.24959887471651143 ) ) ;
#15250 = CARTESIAN_POINT ( 'NONE',  ( 281.2440776823445390, 269.1689414351990308, -150.0938770989752413 ) ) ;
#15251 = EDGE_CURVE ( 'NONE', #8656, #3512, #1927, .T. ) ;
#15252 = CONICAL_SURFACE ( 'NONE', #12578, 2.041999999999999815, 1.047197551196591858 ) ;
#15253 = VERTEX_POINT ( 'NONE', #2450 ) ;
#15254 = AXIS2_PLACEMENT_3D ( 'NONE', #22527, #20860, #13181 ) ;
#15255 = CARTESIAN_POINT ( 'NONE',  ( 0.000000000000000000, -1.178949249685214307, 2.042000000000001592 ) ) ;
#15256 = VERTEX_POINT ( 'NONE', #17077 ) ;
#15257 = FACE_BOUND ( 'NONE', #23611, .T. ) ;
#15258 = ORIENTED_EDGE ( 'NONE', *, *, #7243, .F. ) ;
#15259 = VECTOR ( 'NONE', #357, 1000.000000000000000 ) ;
#15260 = FACE_OUTER_BOUND ( 'NONE', #5873, .T. ) ;
#15261 = SURFACE_SIDE_STYLE ('',( #15379 ) ) ;
#15262 = ITEM_DEFINED_TRANSFORMATION ( 'NONE', 'NONE', #3083,  #11210 ) ;
#15263 = VERTEX_POINT ( 'NONE', #15046 ) ;
#15264 = DIRECTION ( 'NONE',  ( 0.000000000000000000, -3.495664435217746987E-15, -1.000000000000000000 ) ) ;
#15265 = VERTEX_POINT ( 'NONE', #5960 ) ;
#15266 = CARTESIAN_POINT ( 'NONE',  ( -45.00000000000000000, 269.9999999999999432, 0.000000000000000000 ) ) ;
#15267 = CARTESIAN_POINT ( 'NONE',  ( 0.000000000000000000, -2.357898499370432166, 3.035766082959412415E-15 ) ) ;
#15268=STYLED_ITEM('',(#23927),#4664);
#15269 = FACE_BOUND ( 'NONE', #8534, .T. ) ;
#15270 = CLOSED_SHELL ( 'NONE', ( #7808, #4995, #8754, #322, #18206, #3349, #2514, #5367, #17101, #9287, #20952, #6884, #510, #13211, #20696, #705, #11964, #10503, #1242, #21809, #22216, #6797, #22607, #7588, #3823, #20817, #11823 ) ) ;
#15271 = DIRECTION ( 'NONE',  ( 1.776356839400250465E-15, 1.000000000000000000, -3.546545773108138379E-15 ) ) ;
#15272 = VERTEX_POINT ( 'NONE', #7897 ) ;
#15273 = CARTESIAN_POINT ( 'NONE',  ( -280.2488155364688964, 272.8646579186752774, -146.3610889986682650 ) ) ;
#15274 = SHAPE_REPRESENTATION_RELATIONSHIP ( 'NONE' , 'NONE' ,  #2341, #22822 ) ;
#15276 = ORIENTED_EDGE ( 'NONE', *, *, #14090, .F. ) ;
#15275 = EDGE_LOOP ( 'NONE', ( #836, #10277, #10758, #4751 ) ) ;
#15277 = DIRECTION ( 'NONE',  ( 4.862939117679700002E-15, -5.011346215908450209E-15, -1.000000000000000000 ) ) ;
#15278 = EDGE_CURVE ( 'NONE', #17629, #4760, #4276, .T. ) ;
#15279 = FACE_BOUND ( 'NONE', #21595, .T. ) ;
#15280 = CIRCLE ( 'NONE', #17197, 2.100000000000000089 ) ;
#15281 = CARTESIAN_POINT ( 'NONE',  ( 5.000000000000000000, 0.000000000000000000, 0.000000000000000000 ) ) ;
#15282 = EDGE_CURVE ( 'NONE', #12463, #5386, #1974, .T. ) ;
#15283 = CARTESIAN_POINT ( 'NONE',  ( 285.0938770989752697, 269.1689414351989740, 146.2440776823445958 ) ) ;
#15284 = VECTOR ( 'NONE', #2522, 1000.000000000000000 ) ;
#15285 = LINE ( 'NONE', #177, #16825 ) ;
#15286 = ORIENTED_EDGE ( 'NONE', *, *, #10817, .F. ) ;
#15287 = AXIS2_PLACEMENT_3D ( 'NONE', #13480, #22836, #4258 ) ;
#15288 = CARTESIAN_POINT ( 'NONE',  ( -6.811257540890722773, 7.416705727137412829, 200.0000120000000265 ) ) ;
#15289 = CARTESIAN_POINT ( 'NONE',  ( 0.000000000000000000, -1000.000000000000000, 138.9999999999999716 ) ) ;
#15290 =( REPRESENTATION_RELATIONSHIP ('NONE','NONE', #10127, #2341 ) REPRESENTATION_RELATIONSHIP_WITH_TRANSFORMATION ( #11850 )SHAPE_REPRESENTATION_RELATIONSHIP( ) );
#15291 = FACE_OUTER_BOUND ( 'NONE', #13810, .T. ) ;
#15292 = ORIENTED_EDGE ( 'NONE', *, *, #488, .F. ) ;
#15293 = DIRECTION ( 'NONE',  ( 0.000000000000000000, 0.000000000000000000, 1.000000000000000000 ) ) ;
#15294 = ORIENTED_EDGE ( 'NONE', *, *, #10080, .T. ) ;
#15295 = DIRECTION ( 'NONE',  ( -0.000000000000000000, -1.000000000000000000, 0.000000000000000000 ) ) ;
#15296 = CYLINDRICAL_SURFACE ( 'NONE', #977, 2.649999999999971934 ) ;
#15297 = VERTEX_POINT ( 'NONE', #5603 ) ;
#15298 = DIRECTION ( 'NONE',  ( 0.000000000000000000, 0.000000000000000000, -1.000000000000000000 ) ) ;
#15299 = VERTEX_POINT ( 'NONE', #22493 ) ;
#15300 = DIRECTION ( 'NONE',  ( -0.000000000000000000, -0.000000000000000000, 1.000000000000000000 ) ) ;
#15301 = CARTESIAN_POINT ( 'NONE',  ( -281.4928932188134922, 267.7999999999999545, 147.1999999999999886 ) ) ;
#15302 = CARTESIAN_POINT ( 'NONE',  ( 0.000000000000000000, -4.685197434473811207, 4.770489558936219510E-15 ) ) ;
#15303 = CARTESIAN_POINT ( 'NONE',  ( -194.7500000000004832, -494.4690652294794404, -29.99999999999322498 ) ) ;
#15304 = CARTESIAN_POINT ( 'NONE',  ( 232.0000000000000568, -557.0000000000000000, 56.99999999999998579 ) ) ;
#15305 = DIRECTION ( 'NONE',  ( -6.982962677686266711E-15, 0.000000000000000000, 1.000000000000000000 ) ) ;
#15306 = DIRECTION ( 'NONE',  ( 1.000000000000000000, 0.000000000000000000, 0.000000000000000000 ) ) ;
#15307 = ORIENTED_EDGE ( 'NONE', *, *, #267, .T. ) ;
#15308 = SHAPE_REPRESENTATION_RELATIONSHIP ( 'NONE' , 'NONE' ,  #5587, #6714 ) ;
#15309 = FACE_OUTER_BOUND ( 'NONE', #23743, .T. ) ;
#15310 = FACE_OUTER_BOUND ( 'NONE', #4151, .T. ) ;
#15311 = EDGE_LOOP ( 'NONE', ( #105, #3092, #23279, #11381, #17316 ) ) ;
#15312 = ORIENTED_EDGE ( 'NONE', *, *, #14604, .F. ) ;
#15313 = DIRECTION ( 'NONE',  ( -3.736327486719275871E-16, 1.000000000000000000, 0.000000000000000000 ) ) ;
#15314 = CARTESIAN_POINT ( 'NONE',  ( -24.99999999999998224, -52.79999999999944293, 125.0000000000001990 ) ) ;
#15315 = AXIS2_PLACEMENT_3D ( 'NONE', #15854, #21378, #10069 ) ;
#15316 = CARTESIAN_POINT ( 'NONE',  ( 45.00000000000000000, 269.9999999999999432, -5.249999999999973355 ) ) ;
#15317 = ORIENTED_EDGE ( 'NONE', *, *, #2196, .F. ) ;
#15318 = FACE_OUTER_BOUND ( 'NONE', #14332, .T. ) ;
#15319 = CARTESIAN_POINT ( 'NONE',  ( 50.00000000000000000, 0.000000000000000000, 0.000000000000000000 ) ) ;
#15320 = CARTESIAN_POINT ( 'NONE',  ( 158.0000000000000284, -500.0000000000000000, -29.99999999999997158 ) ) ;
#15321 = EDGE_LOOP ( 'NONE', ( #14607, #16460, #5833, #18908, #16247 ) ) ;
#15322 = DIRECTION ( 'NONE',  ( -1.000000000000000000, 3.495664435217746592E-15, -0.000000000000000000 ) ) ;
#15323 = LINE ( 'NONE', #17015, #19212 ) ;
#15324 = VERTEX_POINT ( 'NONE', #9479 ) ;
#15325 = CIRCLE ( 'NONE', #4102, 2.055000000000001492 ) ;
#15326 = CARTESIAN_POINT ( 'NONE',  ( 282.1999999999999318, 268.0880230824753312, -146.3684665479254932 ) ) ;
#15327 = PRODUCT_DEFINITION_SHAPE ( 'NONE', 'NONE',  #23884 ) ;
#15328 = ITEM_DEFINED_TRANSFORMATION ( 'NONE', 'NONE', #5379,  #11210 ) ;
#15329 = PLANE ( 'NONE',  #8907 ) ;
#15330 = VECTOR ( 'NONE', #8097, 1000.000000000000000 ) ;
#15331 = CARTESIAN_POINT ( 'NONE',  ( 2.500000000000000000, 1.768423874527822681, -1.021000000000002794 ) ) ;
#15332 = CARTESIAN_POINT ( 'NONE',  ( -90.00000000000000000, -149.9999999999996874, 129.9038105676659711 ) ) ;
#15333 = VERTEX_POINT ( 'NONE', #11314 ) ;
#15334 = EDGE_LOOP ( 'NONE', ( #3566, #8205, #19355, #1682, #21803 ) ) ;
#15335 = CYLINDRICAL_SURFACE ( 'NONE', #18389, 2.649999999999985700 ) ;
#15336 = CARTESIAN_POINT ( 'NONE',  ( -31.74999999999994316, 0.000000000000000000, 0.000000000000000000 ) ) ;
#15337 = EDGE_CURVE ( 'NONE', #11181, #1699, #20067, .T. ) ;
#15338 = EDGE_CURVE ( 'NONE', #22067, #22845, #4134, .T. ) ;
#15339 = EDGE_CURVE ( 'NONE', #3444, #679, #9595, .T. ) ;
#15340 = AXIS2_PLACEMENT_3D ( 'NONE', #1650, #20232, #9276 ) ;
#15341 = ORIENTED_EDGE ( 'NONE', *, *, #21541, .F. ) ;
#15342 = LINE ( 'NONE', #9908, #17963 ) ;
#15343 = CARTESIAN_POINT ( 'NONE',  ( -127.5319552722390739, 88.09441757049741284, 32.42079297023035878 ) ) ;
#15344 = ORIENTED_EDGE ( 'NONE', *, *, #20757, .F. ) ;
#15345 = LINE ( 'NONE', #5905, #2897 ) ;
#15346 = EDGE_CURVE ( 'NONE', #14427, #2037, #19109, .T. ) ;
#15347 = VECTOR ( 'NONE', #16442, 1000.000000000000000 ) ;
#15348 = EDGE_LOOP ( 'NONE', ( #3448, #3194 ) ) ;
#15349 = FACE_OUTER_BOUND ( 'NONE', #22595, .T. ) ;
#15350 = DIRECTION ( 'NONE',  ( 0.000000000000000000, 1.000000000000000000, 1.177509268541832635E-16 ) ) ;
#15351 = ORIENTED_EDGE ( 'NONE', *, *, #13701, .F. ) ;
#15352 = VERTEX_POINT ( 'NONE', #12154 ) ;
#15353 = CARTESIAN_POINT ( 'NONE',  ( -49.99999999999996447, -59.79999999999975557, 74.99940828143398619 ) ) ;
#15354 = DIRECTION ( 'NONE',  ( 0.000000000000000000, 0.000000000000000000, -1.000000000000000000 ) ) ;
#15355 = LINE ( 'NONE', #4227, #7870 ) ;
#15356 = AXIS2_PLACEMENT_3D ( 'NONE', #12303, #3077, #802 ) ;
#15357 = DIRECTION ( 'NONE',  ( 0.000000000000000000, 0.000000000000000000, 1.000000000000000000 ) ) ;
#15358 = DIRECTION ( 'NONE',  ( 0.000000000000000000, 2.618450529776313049E-15, 1.000000000000000000 ) ) ;
#15359 = FACE_OUTER_BOUND ( 'NONE', #22719, .T. ) ;
#15360 = ORIENTED_EDGE ( 'NONE', *, *, #7190, .F. ) ;
#15361 = DIRECTION ( 'NONE',  ( 0.000000000000000000, 1.000000000000000000, -1.224646799147353207E-16 ) ) ;
#15362 = AXIS2_PLACEMENT_3D ( 'NONE', #17559, #8387, #12533 ) ;
#15363 = VECTOR ( 'NONE', #1950, 1000.000000000000000 ) ;
#15364 = ORIENTED_EDGE ( 'NONE', *, *, #12569, .F. ) ;
#15365 = DIRECTION ( 'NONE',  ( 0.000000000000000000, 0.000000000000000000, -1.000000000000000000 ) ) ;
#15366 = CARTESIAN_POINT ( 'NONE',  ( -2.100000000000000089, 2.571758278209441957E-16, -0.2800830152838844622 ) ) ;
#15367 = ORIENTED_EDGE ( 'NONE', *, *, #15248, .F. ) ;
#15368 = EDGE_CURVE ( 'NONE', #23662, #21209, #14696, .T. ) ;
#15369 = DIRECTION ( 'NONE',  ( 1.000000000000000000, 0.000000000000000000, 0.000000000000000000 ) ) ;
#15370 = ORIENTED_EDGE ( 'NONE', *, *, #17309, .F. ) ;
#15371 = DIRECTION ( 'NONE',  ( -0.000000000000000000, -0.000000000000000000, -1.000000000000000000 ) ) ;
#15372 = EDGE_CURVE ( 'NONE', #13252, #22418, #769, .T. ) ;
#15373 = DIRECTION ( 'NONE',  ( -0.000000000000000000, -0.000000000000000000, -1.000000000000000000 ) ) ;
#15374 = EDGE_CURVE ( 'NONE', #9321, #15709, #17001, .T. ) ;
#15375 = ORIENTED_EDGE ( 'NONE', *, *, #16074, .T. ) ;
#15376 = AXIS2_PLACEMENT_3D ( 'NONE', #21157, #2793, #1104 ) ;
#15377 = CARTESIAN_POINT ( 'NONE',  ( -37.61698748598617215, 140.0355749532209586, 90.00000000000000000 ) ) ;
#15378 = AXIS2_PLACEMENT_3D ( 'NONE', #6251, #11602, #22786 ) ;
#15379 = SURFACE_STYLE_FILL_AREA ( #21031 ) ;
#15380 = AXIS2_PLACEMENT_3D ( 'NONE', #2137, #20372, #9528 ) ;
#15381 = ORIENTED_EDGE ( 'NONE', *, *, #13287, .F. ) ;
#15382 = VECTOR ( 'NONE', #15083, 1000.000000000000000 ) ;
#15383 = EDGE_CURVE ( 'NONE', #14205, #20274, #6565, .T. ) ;
#15384 = CARTESIAN_POINT ( 'NONE',  ( 235.0000000000000284, -560.0000000000000000, -60.00000000000000711 ) ) ;
#15385 = CARTESIAN_POINT ( 'NONE',  ( 0.2500000000000002220, 0.000000000000000000, 4.250000000000021316 ) ) ;
#15386 = DIRECTION ( 'NONE',  ( 1.000000000000000000, 0.000000000000000000, 0.000000000000000000 ) ) ;
#15387 = DIRECTION ( 'NONE',  ( -0.9396926207859143121, 0.000000000000000000, -0.3420201433256525592 ) ) ;
#15388 = VERTEX_POINT ( 'NONE', #19226 ) ;
#15389 = CARTESIAN_POINT ( 'NONE',  ( -280.9952621458755857, 270.4339272673397545, -149.5699028110927600 ) ) ;
#15390 =( NAMED_UNIT ( * ) PLANE_ANGLE_UNIT ( ) SI_UNIT ( $, .RADIAN. ) );
#15392 = ORIENTED_EDGE ( 'NONE', *, *, #19738, .T. ) ;
#15391 = EDGE_LOOP ( 'NONE', ( #10141, #9095, #5070, #12881 ) ) ;
#15393 = VECTOR ( 'NONE', #8199, 1000.000000000000000 ) ;
#15394 = DIRECTION ( 'NONE',  ( -5.050510105632271307E-15, 4.822252111914687128E-15, -1.000000000000000000 ) ) ;
#15395 = AXIS2_PLACEMENT_3D ( 'NONE', #3676, #14708, #14468 ) ;
#15396 = DIRECTION ( 'NONE',  ( -0.000000000000000000, -0.000000000000000000, 1.000000000000000000 ) ) ;
#15397 = CARTESIAN_POINT ( 'NONE',  ( 132.2605194320663600, 80.82189108482278073, -32.24903484778817386 ) ) ;
#15398 = CIRCLE ( 'NONE', #19228, 20.00000000000000000 ) ;
#15399 = VECTOR ( 'NONE', #16741, 1000.000000000000000 ) ;
#15400 = CIRCLE ( 'NONE', #1866, 23.97500000000000497 ) ;
#15401 = CARTESIAN_POINT ( 'NONE',  ( 279.9999999999999432, 269.9999999999999432, 145.0000000000000284 ) ) ;
#15402 = CARTESIAN_POINT ( 'NONE',  ( -284.5699028110928452, 270.4339272673396977, -145.9952621458756141 ) ) ;
#15403 = VERTEX_POINT ( 'NONE', #22965 ) ;
#15404 = AXIS2_PLACEMENT_3D ( 'NONE', #19624, #1395, #3317 ) ;
#15405 = DIRECTION ( 'NONE',  ( 0.000000000000000000, -0.000000000000000000, 1.000000000000000000 ) ) ;
#15406 = CARTESIAN_POINT ( 'NONE',  ( 0.000000000000000000, -1000.000000000000000, -90.00000000000000000 ) ) ;
#15407 = CARTESIAN_POINT ( 'NONE',  ( 112.7436279071518612, 91.18044947429076785, -90.00000000000000000 ) ) ;
#15408 = ORIENTED_EDGE ( 'NONE', *, *, #6365, .T. ) ;
#15409 = CARTESIAN_POINT ( 'NONE',  ( -140.0355749532208449, -37.61698748598668374, -90.00000000000000000 ) ) ;
#15410 = ORIENTED_EDGE ( 'NONE', *, *, #6374, .T. ) ;
#15412 = CARTESIAN_POINT ( 'NONE',  ( 2.500000000000000000, -2.357898499370432166, 3.035766082959412415E-15 ) ) ;
#15411 = AXIS2_PLACEMENT_3D ( 'NONE', #17093, #666, #19128 ) ;
#15413 = FACE_OUTER_BOUND ( 'NONE', #14704, .T. ) ;
#15414 = ADVANCED_FACE ( 'NONE', ( #2704 ), #7356, .T. ) ;
#15415 = ADVANCED_FACE ( 'NONE', ( #6679 ), #6209, .F. ) ;
#15417 = VECTOR ( 'NONE', #21041, 1000.000000000000000 ) ;
#15416 = PRESENTATION_LAYER_ASSIGNMENT (  '', '', ( #15789 ) ) ;
#15418 = EDGE_LOOP ( 'NONE', ( #14184, #15375, #17810, #2278 ) ) ;
#15419 = VECTOR ( 'NONE', #6844, 1000.000000000000000 ) ;
#15420 = ADVANCED_FACE ( 'NONE', ( #10197 ), #4508, .F. ) ;
#15421 = CARTESIAN_POINT ( 'NONE',  ( 5.040301471719072168, 5.750234626350511746, -0.09933465333851003443 ) ) ;
#15422 = VECTOR ( 'NONE', #6234, 1000.000000000000000 ) ;
#15423 = ORIENTED_EDGE ( 'NONE', *, *, #8894, .F. ) ;
#15424 = VECTOR ( 'NONE', #176, 1000.000000000000000 ) ;
#15425 = CARTESIAN_POINT ( 'NONE',  ( -155.0000000000000284, -784.4690652294804067, 27.50000000000647660 ) ) ;
#15426 = VECTOR ( 'NONE', #15602, 1000.000000000000000 ) ;
#15427 = LINE ( 'NONE', #8172, #20730 ) ;
#15428 = DIRECTION ( 'NONE',  ( 0.000000000000000000, 1.000000000000000000, -1.224646799147353207E-16 ) ) ;
#15429 = DIRECTION ( 'NONE',  ( -0.9423651898111408132, -0.3345860861306287348, 6.982962677686266711E-15 ) ) ;
#15430 = DIRECTION ( 'NONE',  ( 0.000000000000000000, -0.4999999999999991118, 0.8660254037844391517 ) ) ;
#15431 = CARTESIAN_POINT ( 'NONE',  ( -1.500000000000000000, 0.000000000000000000, 200.0000000000000000 ) ) ;
#15432 = CARTESIAN_POINT ( 'NONE',  ( -24.83884780301427497, 3.272451888078296012, 145.0000119999999697 ) ) ;
#15433 =( REPRESENTATION_RELATIONSHIP ('NONE','NONE', #10127, #4815 ) REPRESENTATION_RELATIONSHIP_WITH_TRANSFORMATION ( #11613 )SHAPE_REPRESENTATION_RELATIONSHIP( ) );
#15434 = ORIENTED_EDGE ( 'NONE', *, *, #9516, .F. ) ;
#15435 = ITEM_DEFINED_TRANSFORMATION ( 'NONE', 'NONE', #20416,  #11210 ) ;
#15436 = CARTESIAN_POINT ( 'NONE',  ( 90.00000000000000000, 2.914335439641035919E-13, 129.9038105676659711 ) ) ;
#15437 = DIRECTION ( 'NONE',  ( -0.000000000000000000, 1.000000000000000000, -0.000000000000000000 ) ) ;
#15438 = EDGE_LOOP ( 'NONE', ( #18578, #20437 ) ) ;
#15439 = ORIENTED_EDGE ( 'NONE', *, *, #1729, .T. ) ;
#15440 = CARTESIAN_POINT ( 'NONE',  ( 1.499998969197076093, 9.887698300110391969, 200.0000060000000133 ) ) ;
#15441 = DIRECTION ( 'NONE',  ( 0.6964005597823107463, -0.7176533009294141507, 6.982962677686266711E-15 ) ) ;
#15443 = CONICAL_SURFACE ( 'NONE', #6555, 5.560781378645573980, 1.221730476396046816 ) ;
#15442 = AXIS2_PLACEMENT_3D ( 'NONE', #15630, #22962, #11793 ) ;
#15444 = VECTOR ( 'NONE', #13728, 1000.000000000000000 ) ;
#15445 = VECTOR ( 'NONE', #16086, 1000.000000000000000 ) ;
#15446 = DIRECTION ( 'NONE',  ( 0.000000000000000000, -1.000000000000000000, 1.103561164596346103E-15 ) ) ;
#15447 = CIRCLE ( 'NONE', #15821, 145.0000000000000284 ) ;
#15448 = ORIENTED_EDGE ( 'NONE', *, *, #8789, .F. ) ;
#15449 = DIRECTION ( 'NONE',  ( 0.000000000000000000, 0.000000000000000000, 1.000000000000000000 ) ) ;
#15450 = CARTESIAN_POINT ( 'NONE',  ( 5.200000000000002842, 0.000000000000000000, 0.000000000000000000 ) ) ;
#15451 = CARTESIAN_POINT ( 'NONE',  ( 2.500000000000000000, -1.768423874527824902, -1.020999999999998353 ) ) ;
#15452 = ORIENTED_EDGE ( 'NONE', *, *, #22406, .F. ) ;
#15453 = CARTESIAN_POINT ( 'NONE',  ( 280.4357574145958552, 272.4730547946948036, 147.3059783239181115 ) ) ;
#15454 = DIRECTION ( 'NONE',  ( -1.000000000000000000, -0.000000000000000000, -0.000000000000000000 ) ) ;
#15455 = EDGE_CURVE ( 'NONE', #5390, #9249, #12052, .T. ) ;
#15456 = FACE_BOUND ( 'NONE', #6142, .T. ) ;
#15457 = VERTEX_POINT ( 'NONE', #15744 ) ;
#15458 = DIRECTION ( 'NONE',  ( 4.625929269271484928E-16, -3.469446951953613794E-15, -1.000000000000000000 ) ) ;
#15459 = ITEM_DEFINED_TRANSFORMATION ( 'NONE', 'NONE', #12383,  #11210 ) ;
#15460 = EDGE_CURVE ( 'NONE', #1219, #6867, #21294, .T. ) ;
#15461 = CARTESIAN_POINT ( 'NONE',  ( -281.4928932188134354, -127.0000000000000568, -152.4000000000012847 ) ) ;
#15462 = CARTESIAN_POINT ( 'NONE',  ( -280.0000000000000568, 269.9999999999999432, 145.0000000000000284 ) ) ;
#15463 = B_SPLINE_CURVE_WITH_KNOTS ( 'NONE', 3,
 ( #496, #15125, #16911, #19393, #15805, #4686, #13445, #18948, #2851, #22570, #2410, #13904, #9799, #7744, #17156, #612, #10253, #23151, #6618, #17592, #22454, #14011, #21340, #8554, #15922, #23258, #6730, #14126, #14577, #22044, #14707, #10976, #10869, #5504 ),
 .UNSPECIFIED., .F., .F.,
 ( 4, 2, 2, 2, 2, 2, 2, 2, 2, 2, 2, 2, 2, 2, 2, 2, 4 ),
 ( 0.7500000000000000000, 0.7812500000000000000, 0.8125000000000000000, 0.8437500000000000000, 0.8750000000000000000, 0.9062500000000000000, 0.9375000000000000000, 0.9687500000000000000, 1.000000000000000000, 1.031250000000000000, 1.062500000000000000, 1.093750000000000000, 1.125000000000000000, 1.156250000000000000, 1.187500000000000000, 1.218750000000000000, 1.250000000000000000 ),
 .UNSPECIFIED. ) ;
#15464 = CARTESIAN_POINT ( 'NONE',  ( 312.2000000000013529, -132.2000000000000455, 0.000000000000000000 ) ) ;
#15465 = AXIS2_PLACEMENT_3D ( 'NONE', #3188, #21565, #21679 ) ;
#15466 = DIRECTION ( 'NONE',  ( -1.000000000000000000, -0.000000000000000000, -0.000000000000000000 ) ) ;
#15467 = AXIS2_PLACEMENT_3D ( 'NONE', #15921, #23257, #4443 ) ;
#15468 = VERTEX_POINT ( 'NONE', #8149 ) ;
#15469 = EDGE_LOOP ( 'NONE', ( #4925, #5660, #2524, #4448 ) ) ;
#15470 = FACE_OUTER_BOUND ( 'NONE', #4480, .T. ) ;
#15471 = CARTESIAN_POINT ( 'NONE',  ( 2.500000000000000000, -1.178949249685214307, 2.042000000000001592 ) ) ;
#15472 = VERTEX_POINT ( 'NONE', #15522 ) ;
#15473 = CYLINDRICAL_SURFACE ( 'NONE', #20997, 2.199999999999979750 ) ;
#15474 = CARTESIAN_POINT ( 'NONE',  ( 45.00000000000004974, -52.79999999999967031, 50.00000000000018474 ) ) ;
#15475 = CYLINDRICAL_SURFACE ( 'NONE', #10371, 24.99999999999998224 ) ;
#15476 = ORIENTED_EDGE ( 'NONE', *, *, #8980, .F. ) ;
#15477 = DIRECTION ( 'NONE',  ( -0.8090169943749428993, -0.5877852522924793544, 0.000000000000000000 ) ) ;
#15478 = EDGE_CURVE ( 'NONE', #19715, #1956, #17433, .T. ) ;
#15479 = EDGE_LOOP ( 'NONE', ( #950, #20525, #5113, #19595 ) ) ;
#15480 = CARTESIAN_POINT ( 'NONE',  ( -44.99999999999995026, -56.79999999999970584, 47.35000000000020037 ) ) ;
#15481 = CARTESIAN_POINT ( 'NONE',  ( 312.2000000000013529, -132.2000000000000455, -146.4928932188134070 ) ) ;
#15482 = VERTEX_POINT ( 'NONE', #4742 ) ;
#15483 = EDGE_LOOP ( 'NONE', ( #16856, #465, #17390 ) ) ;
#15484 = CARTESIAN_POINT ( 'NONE',  ( 1.274258131564866448, 3.883108878240963513, -3.220599429844046568 ) ) ;
#15485 = PRODUCT_DEFINITION_SHAPE ( 'NONE', 'NONE',  #23869 ) ;
#15486 = DIRECTION ( 'NONE',  ( 0.000000000000000000, -0.5000000000000011102, -0.8660254037844379305 ) ) ;
#15487 = EDGE_CURVE ( 'NONE', #13550, #17898, #8369, .T. ) ;
#15488 = DIRECTION ( 'NONE',  ( -1.000000000000000000, 0.000000000000000000, 0.000000000000000000 ) ) ;
#15489 = CARTESIAN_POINT ( 'NONE',  ( -281.4928932188135491, -129.2000000000000455, 177.2000000000014097 ) ) ;
#15490 = ORIENTED_EDGE ( 'NONE', *, *, #23146, .T. ) ;
#15491 = CARTESIAN_POINT ( 'NONE',  ( 10.40000000000000036, 6.613092715395709439E-16, 5.400000000000002132 ) ) ;
#15492 =( NAMED_UNIT ( * ) SI_UNIT ( $, .STERADIAN. ) SOLID_ANGLE_UNIT ( ) );
#15493 = EDGE_CURVE ( 'NONE', #10493, #13502, #2803, .T. ) ;
#15494 = B_SPLINE_CURVE_WITH_KNOTS ( 'NONE', 3,
 ( #8502, #12271, #19574, #10926, #23800, #14534, #20174, #14656 ),
 .UNSPECIFIED., .F., .F.,
 ( 4, 2, 2, 4 ),
 ( 0.005725059856848645212, 0.006314084072593634418, 0.006903108288338624492, 0.008081156719828603771 ),
 .UNSPECIFIED. ) ;
#15495 = ORIENTED_EDGE ( 'NONE', *, *, #5134, .T. ) ;
#15496 = CARTESIAN_POINT ( 'NONE',  ( -146.4450000000005332, -204.4690652294800657, -32.49999999999356248 ) ) ;
#15497 = EDGE_LOOP ( 'NONE', ( #22229, #6994, #8168, #7061 ) ) ;
#15498 = CARTESIAN_POINT ( 'NONE',  ( -24.99995073930943690, -1.642023387880738428, -145.0000000000000284 ) ) ;
#15499 = ORIENTED_EDGE ( 'NONE', *, *, #13067, .T. ) ;
#15500 = B_SPLINE_CURVE_WITH_KNOTS ( 'NONE', 3,
 ( #8631, #8758, #8522, #16119, #21420, #14336, #12290, #21665, #5123, #12531, #22239, #18728, #5591, #9466, #13002, #16818, #5356, #5837, #22117, #20303 ),
 .UNSPECIFIED., .F., .F.,
 ( 4, 2, 2, 2, 2, 2, 2, 2, 2, 4 ),
 ( 0.000000000000000000, 0.001035985217005782819, 0.002071970434011565637, 0.003107955651017348889, 0.003625948259520284968, 0.004143940868023221480, 0.005179926085028920164, 0.006215911302034618849, 0.007251896519040319268, 0.008287881736046017953 ),
 .UNSPECIFIED. ) ;
#15501 = CARTESIAN_POINT ( 'NONE',  ( 7.500000000000000000, -3.608439182435168036, -7.298562697733107285 ) ) ;
#15502 = LINE ( 'NONE', #4722, #21801 ) ;
#15503 = ORIENTED_EDGE ( 'NONE', *, *, #6954, .T. ) ;
#15504 = CARTESIAN_POINT ( 'NONE',  ( -280.4976310729379065, 269.7223300543793698, 146.1079617568159961 ) ) ;
#15505 = FILL_AREA_STYLE ('',( #17301 ) ) ;
#15506 = ORIENTED_EDGE ( 'NONE', *, *, #9187, .F. ) ;
#15507 = UNCERTAINTY_MEASURE_WITH_UNIT (LENGTH_MEASURE( 1.000000000000000082E-05 ), #3325, 'distance_accuracy_value', 'NONE');
#15508 = EDGE_CURVE ( 'NONE', #21395, #1131, #18910, .T. ) ;
#15509 = DIRECTION ( 'NONE',  ( 0.000000000000000000, 0.4999999999999993339, -0.8660254037844390407 ) ) ;
#15510 = EDGE_CURVE ( 'NONE', #1352, #17167, #15494, .T. ) ;
#15511 = CARTESIAN_POINT ( 'NONE',  ( -3.266795291543685309, -975.1599768041793368, -145.0000000000001137 ) ) ;
#15512 = CARTESIAN_POINT ( 'NONE',  ( -5.276765049035075705, 6.073111908730296271, -7.634085501268424778 ) ) ;
#15513 = DIRECTION ( 'NONE',  ( 2.238759164535664589E-46, 3.469446951953614189E-15, 1.000000000000000000 ) ) ;
#15514 = ORIENTED_EDGE ( 'NONE', *, *, #5849, .F. ) ;
#15515 = CARTESIAN_POINT ( 'NONE',  ( 0.000000000000000000, 0.000000000000000000, 20.00000000000000000 ) ) ;
#15516 = EDGE_CURVE ( 'NONE', #22350, #20294, #6866, .T. ) ;
#15517 = ADVANCED_FACE ( 'NONE', ( #19710 ), #8975, .T. ) ;
#15519 = ORIENTED_EDGE ( 'NONE', *, *, #2838, .T. ) ;
#15518 = ORIENTED_EDGE ( 'NONE', *, *, #2839, .F. ) ;
#15520 = DIRECTION ( 'NONE',  ( 0.9423651898111408132, 0.3345860861306287348, -6.982962677686266711E-15 ) ) ;
#15521 = CARTESIAN_POINT ( 'NONE',  ( 7.500000000000000000, 4.732328341851997244, -7.493855119309152713 ) ) ;
#15522 = CARTESIAN_POINT ( 'NONE',  ( 1.500000000000000000, 9.886859966642592923, -50.00000000000000000 ) ) ;
#15523 = EDGE_CURVE ( 'NONE', #4045, #13958, #21869, .T. ) ;
#15524 = CARTESIAN_POINT ( 'NONE',  ( -45.24999999999994316, 100.0000000000000000, 145.0000000000000000 ) ) ;
#15525 = CARTESIAN_POINT ( 'NONE',  ( -280.2840560642353012, 269.9696999999999889, -145.1244266425809712 ) ) ;
#15526 = ORIENTED_EDGE ( 'NONE', *, *, #10514, .T. ) ;
#15527 = EDGE_CURVE ( 'NONE', #16945, #3284, #12410, .T. ) ;
#15528 = DIRECTION ( 'NONE',  ( 0.000000000000000000, 0.000000000000000000, 1.000000000000000000 ) ) ;
#15529 = FACE_OUTER_BOUND ( 'NONE', #1777, .T. ) ;
#15530 = CARTESIAN_POINT ( 'NONE',  ( 122.9560050114707934, -1094.375960373423595, 30.32918505548578381 ) ) ;
#15531 = CONTEXT_DEPENDENT_SHAPE_REPRESENTATION ( #2906, #3313 ) ;
#15532 = ORIENTED_EDGE ( 'NONE', *, *, #619, .F. ) ;
#15533 = VECTOR ( 'NONE', #3937, 1000.000000000000000 ) ;
#15534 = DIRECTION ( 'NONE',  ( 0.000000000000000000, -1.000000000000000000, 6.123233995736766036E-17 ) ) ;
#15535 = VERTEX_POINT ( 'NONE', #23330 ) ;
#15536 = DIRECTION ( 'NONE',  ( -0.000000000000000000, -0.000000000000000000, -1.000000000000000000 ) ) ;
#15537 = CARTESIAN_POINT ( 'NONE',  ( 7.499999999999997335, 34.18698582794336005, -100.0000000000000000 ) ) ;
#15538 = ORIENTED_EDGE ( 'NONE', *, *, #10905, .F. ) ;
#15539 = CARTESIAN_POINT ( 'NONE',  ( -3.266795292121510208, 24.84002319558113214, -145.0000000000000000 ) ) ;
#15540 = ORIENTED_EDGE ( 'NONE', *, *, #13093, .F. ) ;
#15541 = SURFACE_SIDE_STYLE ('',( #8278 ) ) ;
#15542 = DIRECTION ( 'NONE',  ( 1.000000000000000000, 0.000000000000000000, 0.000000000000000000 ) ) ;
#15543 = DIRECTION ( 'NONE',  ( 1.000000000000000000, 0.000000000000000000, 0.000000000000000000 ) ) ;
#15544 = CARTESIAN_POINT ( 'NONE',  ( 0.000000000000000000, 0.000000000000000000, -100.0000000000000000 ) ) ;
#15545 = ADVANCED_FACE ( 'NONE', ( #12871 ), #10809, .F. ) ;
#15546 = PLANE ( 'NONE',  #8438 ) ;
#15547 = LINE ( 'NONE', #8283, #7308 ) ;
#15548 = EDGE_CURVE ( 'NONE', #5262, #7318, #5689, .T. ) ;
#15549 = LINE ( 'NONE', #1151, #15187 ) ;
#15550 = EDGE_LOOP ( 'NONE', ( #1411, #17964, #5998, #23463 ) ) ;
#15551 = SHAPE_REPRESENTATION_RELATIONSHIP ( 'NONE' , 'NONE' ,  #8987, #6409 ) ;
#15552 = ADVANCED_FACE ( 'NONE', ( #16233 ), #6085, .F. ) ;
#15553 = CARTESIAN_POINT ( 'NONE',  ( -287.4000000000014552, -127.0000000000000568, 146.4928932188134638 ) ) ;
#15554 = CARTESIAN_POINT ( 'NONE',  ( -4.203934362469166963, -1.640673743454851286, -3.598432614606932756 ) ) ;
#15555 = EDGE_LOOP ( 'NONE', ( #4862, #18953, #3390, #13240 ) ) ;
#15556 = AXIS2_PLACEMENT_3D ( 'NONE', #13303, #8080, #4069 ) ;
#15557 = ORIENTED_EDGE ( 'NONE', *, *, #3076, .F. ) ;
#15558 = CARTESIAN_POINT ( 'NONE',  ( -64.99999999999998579, -52.79999999999942872, 125.0000000000001421 ) ) ;
#15559 = CARTESIAN_POINT ( 'NONE',  ( 40.00000000000000000, 100.0000000000000000, 150.2000000000009550 ) ) ;
#15560 = EDGE_CURVE ( 'NONE', #14084, #7880, #23577, .T. ) ;
#15561 = ADVANCED_FACE ( 'NONE', ( #12516 ), #18249, .T. ) ;
#15562 = PLANE ( 'NONE',  #13343 ) ;
#15563 = CARTESIAN_POINT ( 'NONE',  ( 1.500000000000000000, 12.00000000000000000, 0.000000000000000000 ) ) ;
#15564 = CARTESIAN_POINT ( 'NONE',  ( 45.00000000000004974, -52.79999999999967741, 47.35000000000019327 ) ) ;
#15565 = DIRECTION ( 'NONE',  ( 0.000000000000000000, 0.000000000000000000, 1.000000000000000000 ) ) ;
#15566 = EDGE_LOOP ( 'NONE', ( #14168, #8340, #5415, #8559 ) ) ;
#15567 = DIRECTION ( 'NONE',  ( -1.000000000000000000, 1.408839003528726857E-14, 6.982962677686266711E-15 ) ) ;
#15568 = CARTESIAN_POINT ( 'NONE',  ( -0.6666666666666666297, -4.233901974057276973, -3.300726591567087365 ) ) ;
#15569 = ORIENTED_EDGE ( 'NONE', *, *, #13204, .F. ) ;
#15570 = DIRECTION ( 'NONE',  ( 0.000000000000000000, 1.177509268541832635E-16, -1.000000000000000000 ) ) ;
#15571 = CIRCLE ( 'NONE', #18607, 4.000000000000000000 ) ;
#15572 = APPLICATION_CONTEXT ( 'automotive_design' ) ;
#15573 = DIRECTION ( 'NONE',  ( -4.862939117679700002E-15, 5.011346215908450209E-15, 1.000000000000000000 ) ) ;
#15574 = CARTESIAN_POINT ( 'NONE',  ( -0.2727178028658734932, 2.936090700955779752E-15, -23.97500000000000497 ) ) ;
#15575 = DIRECTION ( 'NONE',  ( 0.000000000000000000, 0.000000000000000000, -1.000000000000000000 ) ) ;
#15576 = VERTEX_POINT ( 'NONE', #5340 ) ;
#15577 = ORIENTED_EDGE ( 'NONE', *, *, #19488, .T. ) ;
#15578 = DIRECTION ( 'NONE',  ( 1.000000000000000000, -0.000000000000000000, -0.000000000000000000 ) ) ;
#15579 = DIRECTION ( 'NONE',  ( 0.000000000000000000, 0.000000000000000000, -1.000000000000000000 ) ) ;
#15580 = EDGE_LOOP ( 'NONE', ( #8062, #6162, #17326, #9415, #16334 ) ) ;
#15581 = CIRCLE ( 'NONE', #10233, 25.00000000000000000 ) ;
#15582 = AXIS2_PLACEMENT_3D ( 'NONE', #22209, #3971, #22340 ) ;
#15583 = EDGE_CURVE ( 'NONE', #4214, #21432, #14188, .T. ) ;
#15584 = EDGE_CURVE ( 'NONE', #12953, #13741, #10350, .T. ) ;
#15585 = VECTOR ( 'NONE', #11284, 1000.000000000000000 ) ;
#15586 = EDGE_LOOP ( 'NONE', ( #16459, #4098, #4694, #2468 ) ) ;
#15587 = CARTESIAN_POINT ( 'NONE',  ( 280.1244295015774810, 273.0299999999999159, 145.6847249064867356 ) ) ;
#15588 = ADVANCED_FACE ( 'NONE', ( #23449 ), #9090, .T. ) ;
#15589 = LINE ( 'NONE', #11866, #4903 ) ;
#15590 = ORIENTED_EDGE ( 'NONE', *, *, #16734, .F. ) ;
#15591 = CARTESIAN_POINT ( 'NONE',  ( 5.200000000000020606, 0.000000000000000000, -6.938893903907228378E-15 ) ) ;
#15592 = ORIENTED_EDGE ( 'NONE', *, *, #4889, .T. ) ;
#15593 = CARTESIAN_POINT ( 'NONE',  ( -40.00000000000000000, 100.0000000000000000, -150.2000000000005571 ) ) ;
#15594 = FACE_BOUND ( 'NONE', #5426, .T. ) ;
#15595 = ORIENTED_EDGE ( 'NONE', *, *, #6326, .F. ) ;
#15596 = VERTEX_POINT ( 'NONE', #12633 ) ;
#15597 = DIRECTION ( 'NONE',  ( 1.000000000000000000, 0.000000000000000000, 0.000000000000000000 ) ) ;
#15598 = VECTOR ( 'NONE', #9403, 1000.000000000000000 ) ;
#15599 = FACE_OUTER_BOUND ( 'NONE', #3989, .T. ) ;
#15600 = CIRCLE ( 'NONE', #19420, 10.12668159690567649 ) ;
#15601 = FACE_OUTER_BOUND ( 'NONE', #4960, .T. ) ;
#15602 = DIRECTION ( 'NONE',  ( -1.000000000000000000, -0.000000000000000000, -0.000000000000000000 ) ) ;
#15603 = EDGE_LOOP ( 'NONE', ( #21499, #3552, #11310, #2600 ) ) ;
#15604 = DIRECTION ( 'NONE',  ( 0.9289202219288174023, 0.3702799228849933955, 6.982962677686265922E-15 ) ) ;
#15605 = SURFACE_STYLE_FILL_AREA ( #8226 ) ;
#15606 = ORIENTED_EDGE ( 'NONE', *, *, #5166, .F. ) ;
#15607 = ORIENTED_EDGE ( 'NONE', *, *, #23489, .T. ) ;
#15608 = ADVANCED_FACE ( 'NONE', ( #19944 ), #1469, .F. ) ;
#15609=STYLED_ITEM('',(#23927),#12097);
#15610 = CARTESIAN_POINT ( 'NONE',  ( 21.69892645970834621, -12.52401366503153213, -145.0000000000000000 ) ) ;
#15611 = CIRCLE ( 'NONE', #2856, 2.649999999999989253 ) ;
#15612 = EDGE_LOOP ( 'NONE', ( #19078, #4715 ) ) ;
#15613 = DIRECTION ( 'NONE',  ( -0.000000000000000000, -0.000000000000000000, 1.000000000000000000 ) ) ;
#15614 = DIRECTION ( 'NONE',  ( 0.000000000000000000, 1.000000000000000000, 1.177509268541832635E-16 ) ) ;
#15615 = ORIENTED_EDGE ( 'NONE', *, *, #20073, .F. ) ;
#15616 = CARTESIAN_POINT ( 'NONE',  ( -280.8708543776413080, 269.1333820183295416, 146.7350371479513171 ) ) ;
#15617 = DIRECTION ( 'NONE',  ( 0.000000000000000000, -1.000000000000000000, 0.000000000000000000 ) ) ;
#15618 = ORIENTED_EDGE ( 'NONE', *, *, #19927, .F. ) ;
#15619 = CARTESIAN_POINT ( 'NONE',  ( -281.4928932188134922, -127.0000000000000568, -150.2000000000013245 ) ) ;
#15620 = CARTESIAN_POINT ( 'NONE',  ( -21.69895866495090786, -987.4760640919365642, -145.0000000000001421 ) ) ;
#15621 = CARTESIAN_POINT ( 'NONE',  ( -2.623433461001184686, 7.604994000793856124, -7.633824513837113912 ) ) ;
#15622 = SHAPE_REPRESENTATION ( 'support structure', ( #11210 ), #16580 ) ;
#15623 = CIRCLE ( 'NONE', #19443, 4.250000000000000000 ) ;
#15624 = CARTESIAN_POINT ( 'NONE',  ( 25.00000000000000000, 4.926831259382130415E-15, 138.9999999999999716 ) ) ;
#15625 = VERTEX_POINT ( 'NONE', #8613 ) ;
#15626 = DIRECTION ( 'NONE',  ( 1.000000000000000000, 3.469446951953614682E-16, 0.000000000000000000 ) ) ;
#15628 = ORIENTED_EDGE ( 'NONE', *, *, #19447, .T. ) ;
#15627 = ORIENTED_EDGE ( 'NONE', *, *, #14599, .F. ) ;
#15629 = VECTOR ( 'NONE', #6604, 1000.000000000000000 ) ;
#15630 = CARTESIAN_POINT ( 'NONE',  ( -163.0000000000000853, -784.4690652294802931, 30.00000000000653699 ) ) ;
#15631 = CARTESIAN_POINT ( 'NONE',  ( -2.352990130084580066E-16, 8.660254037844390851, -7.422398894150034288 ) ) ;
#15632 = CARTESIAN_POINT ( 'NONE',  ( 7.499999999999999112, 41.99999999999998579, -100.0000000000000000 ) ) ;
#15633 = CYLINDRICAL_SURFACE ( 'NONE', #6160, 2.500000000000000444 ) ;
#15634 = EDGE_CURVE ( 'NONE', #16985, #5557, #18039, .T. ) ;
#15635 = CARTESIAN_POINT ( 'NONE',  ( -281.1079617568159961, 269.7223300543793698, -145.4976310729377929 ) ) ;
#15636 = EDGE_LOOP ( 'NONE', ( #2684, #17120, #9363, #12433 ) ) ;
#15637 = ADVANCED_FACE ( 'NONE', ( #17904 ), #10785, .F. ) ;
#15638 = EDGE_CURVE ( 'NONE', #733, #12117, #20291, .T. ) ;
#15639 = CARTESIAN_POINT ( 'NONE',  ( 126.3653543294811499, 77.28387428943223370, 30.00000000000641620 ) ) ;
#15640 = AXIS2_PLACEMENT_3D ( 'NONE', #23280, #12355, #15829 ) ;
#15641 = CARTESIAN_POINT ( 'NONE',  ( 145.9999999999998010, -801.0618695410399823, 30.00000000000641620 ) ) ;
#15642 = DIRECTION ( 'NONE',  ( 0.000000000000000000, 0.000000000000000000, -1.000000000000000000 ) ) ;
#15643 = EDGE_CURVE ( 'NONE', #9003, #16299, #13460, .T. ) ;
#15644 = EDGE_LOOP ( 'NONE', ( #21797, #13955, #21908, #17181 ) ) ;
#15645 = CIRCLE ( 'NONE', #1351, 4.250000000000000000 ) ;
#15646 = LINE ( 'NONE', #17447, #8671 ) ;
#15647 = ORIENTED_EDGE ( 'NONE', *, *, #18589, .F. ) ;
#15648 = CLOSED_SHELL ( 'NONE', ( #10811, #19496, #4296, #7095, #10319, #22271, #19618, #19485, #13360, #4464, #18769, #23307, #16787, #19526, #14217, #7939, #14225, #1338, #8985, #19033, #9959, #3034, #7098, #23338, #11403, #15756, #23571 ) ) ;
#15649 = FACE_OUTER_BOUND ( 'NONE', #15311, .T. ) ;
#15650 = VERTEX_POINT ( 'NONE', #508 ) ;
#15651 = DIRECTION ( 'NONE',  ( -0.000000000000000000, -0.000000000000000000, -1.000000000000000000 ) ) ;
#15652 = ORIENTED_EDGE ( 'NONE', *, *, #522, .F. ) ;
#15653 = PRESENTATION_STYLE_ASSIGNMENT (( #2932 ) ) ;
#15654 = CARTESIAN_POINT ( 'NONE',  ( -1.654252653721913102, -3.663718938583024443, -0.01223254789874440342 ) ) ;
#15655 = EDGE_CURVE ( 'NONE', #2537, #12825, #4540, .T. ) ;
#15656 = DIRECTION ( 'NONE',  ( 0.000000000000000000, -0.000000000000000000, 1.000000000000000000 ) ) ;
#15657 = CARTESIAN_POINT ( 'NONE',  ( 280.7095819834010513, 269.8873946496626672, 145.3113419039144958 ) ) ;
#15658 = VECTOR ( 'NONE', #23194, 1000.000000000000114 ) ;
#15659 = CYLINDRICAL_SURFACE ( 'NONE', #20807, 5.249999999999942268 ) ;
#15660 = CARTESIAN_POINT ( 'NONE',  ( 45.00000000000000000, 269.9999999999999432, 0.000000000000000000 ) ) ;
#15661 = VERTEX_POINT ( 'NONE', #13107 ) ;
#15662 =( NAMED_UNIT ( * ) SI_UNIT ( $, .STERADIAN. ) SOLID_ANGLE_UNIT ( ) );
#15663 = PLANE ( 'NONE',  #6857 ) ;
#15664 = DIRECTION ( 'NONE',  ( -0.000000000000000000, -0.000000000000000000, 1.000000000000000000 ) ) ;
#15665 = ORIENTED_EDGE ( 'NONE', *, *, #8316, .F. ) ;
#15666 = AXIS2_PLACEMENT_3D ( 'NONE', #8035, #2351, #440 ) ;
#15667 = ORIENTED_EDGE ( 'NONE', *, *, #2575, .T. ) ;
#15668 = CARTESIAN_POINT ( 'NONE',  ( 7.499999999999999112, 41.99999999999998579, -100.0000000000000000 ) ) ;
#15669 = DIRECTION ( 'NONE',  ( -1.000000000000000000, -3.469446951953614682E-16, -0.000000000000000000 ) ) ;
#15670 = ADVANCED_BREP_SHAPE_REPRESENTATION ( '', ( #4664, #11210 ), #9660 ) ;
#15672 = DIRECTION ( 'NONE',  ( -0.000000000000000000, 0.000000000000000000, -1.000000000000000000 ) ) ;
#15671 = PRODUCT_DEFINITION_SHAPE ( 'NONE', 'NONE',  #23866 ) ;
#15673 = DIRECTION ( 'NONE',  ( -1.000000000000000000, 1.408839003528726857E-14, 6.982962677686266711E-15 ) ) ;
#15674 = FACE_OUTER_BOUND ( 'NONE', #12475, .T. ) ;
#15675 = ADVANCED_FACE ( 'NONE', ( #22222 ), #8026, .F. ) ;
#15676 = CARTESIAN_POINT ( 'NONE',  ( -40.00000000000000000, 100.0000000000000000, 125.0000000000000000 ) ) ;
#15677 = EDGE_CURVE ( 'NONE', #4839, #20854, #11516, .T. ) ;
#15678 = ORIENTED_EDGE ( 'NONE', *, *, #9622, .F. ) ;
#15679 = PLANE ( 'NONE',  #4843 ) ;
#15680 = CARTESIAN_POINT ( 'NONE',  ( -145.0000000000000284, -1000.000000000000000, 90.00000000000000000 ) ) ;
#15681 = DIRECTION ( 'NONE',  ( 0.000000000000000000, 0.000000000000000000, -1.000000000000000000 ) ) ;
#15682 = VERTEX_POINT ( 'NONE', #260 ) ;
#15683 = DIRECTION ( 'NONE',  ( -1.000000000000000000, 0.000000000000000000, 0.000000000000000000 ) ) ;
#15684 = EDGE_CURVE ( 'NONE', #20769, #21638, #7614, .T. ) ;
#15685 = ITEM_DEFINED_TRANSFORMATION ( 'NONE', 'NONE', #22351,  #11210 ) ;
#15686 = DIRECTION ( 'NONE',  ( 0.000000000000000000, -0.000000000000000000, -1.000000000000000000 ) ) ;
#15687 = EDGE_CURVE ( 'NONE', #14223, #15996, #2988, .T. ) ;
#15688 = DIRECTION ( 'NONE',  ( 0.000000000000000000, 2.618450529776313049E-15, 1.000000000000000000 ) ) ;
#15689 = CARTESIAN_POINT ( 'NONE',  ( -284.5132312761074331, 270.4054396500289954, 145.9953931959807676 ) ) ;
#15690 = VERTEX_POINT ( 'NONE', #15496 ) ;
#15691 = EDGE_LOOP ( 'NONE', ( #21086, #14984 ) ) ;
#15692 = CARTESIAN_POINT ( 'NONE',  ( -280.4357337430841426, 269.7771650631953548, -145.9755899421581944 ) ) ;
#15693 = AXIS2_PLACEMENT_3D ( 'NONE', #21680, #3780, #23716 ) ;
#15694 = DIRECTION ( 'NONE',  ( -1.000000000000000000, 1.408839003528726857E-14, 6.982962677686266711E-15 ) ) ;
#15695 = DIRECTION ( 'NONE',  ( -0.000000000000000000, 1.000000000000000000, 0.000000000000000000 ) ) ;
#15696 = ORIENTED_EDGE ( 'NONE', *, *, #12405, .F. ) ;
#15697 = CONICAL_SURFACE ( 'NONE', #2936, 2.055000000000001492, 0.7853981633974633780 ) ;
#15698 = VERTEX_POINT ( 'NONE', #14258 ) ;
#15699 = DIRECTION ( 'NONE',  ( 0.000000000000000000, 0.000000000000000000, 1.000000000000000000 ) ) ;
#15700 = DIRECTION ( 'NONE',  ( -0.000000000000000000, -1.000000000000000000, -1.110223024625156540E-16 ) ) ;
#15701 = ORIENTED_EDGE ( 'NONE', *, *, #16399, .T. ) ;
#15702 = CARTESIAN_POINT ( 'NONE',  ( -135.6291186032802614, -1075.032345129803616, -32.49999999999351274 ) ) ;
#15703 = ORIENTED_EDGE ( 'NONE', *, *, #20391, .T. ) ;
#15704 = AXIS2_PLACEMENT_3D ( 'NONE', #3370, #14164, #3497 ) ;
#15705 = CARTESIAN_POINT ( 'NONE',  ( -4.211140560182196957, -2.431303136016552013, -3.745885042887436178 ) ) ;
#15706 = LINE ( 'NONE', #12231, #1296 ) ;
#15707 = AXIS2_PLACEMENT_3D ( 'NONE', #12824, #20126, #3571 ) ;
#15708 = ORIENTED_EDGE ( 'NONE', *, *, #2032, .T. ) ;
#15709 = VERTEX_POINT ( 'NONE', #9810 ) ;
#15710 = LINE ( 'NONE', #6642, #3438 ) ;
#15711 = DIRECTION ( 'NONE',  ( -1.000000000000000000, 0.000000000000000000, 0.000000000000000000 ) ) ;
#15712 = EDGE_CURVE ( 'NONE', #13249, #6476, #6990, .T. ) ;
#15713 = ADVANCED_FACE ( 'NONE', ( #20903 ), #1192, .F. ) ;
#15714 = EDGE_CURVE ( 'NONE', #12957, #640, #10387, .T. ) ;
#15715 = CARTESIAN_POINT ( 'NONE',  ( 145.9999999999998010, -209.9999999999996874, 30.00000000000641620 ) ) ;
#15716 = DIRECTION ( 'NONE',  ( 1.000000000000000000, 0.000000000000000000, 0.000000000000000000 ) ) ;
#15717 = VERTEX_POINT ( 'NONE', #6291 ) ;
#15718 = DIRECTION ( 'NONE',  ( -1.000000000000000000, -0.000000000000000000, -0.000000000000000000 ) ) ;
#15719 = VERTEX_POINT ( 'NONE', #19658 ) ;
#15720 = AXIS2_PLACEMENT_3D ( 'NONE', #18100, #14267, #16296 ) ;
#15721 = ORIENTED_EDGE ( 'NONE', *, *, #19798, .T. ) ;
#15722 = DIRECTION ( 'NONE',  ( -0.000000000000000000, 1.000000000000000000, 0.000000000000000000 ) ) ;
#15723 = ORIENTED_EDGE ( 'NONE', *, *, #13677, .T. ) ;
#15724 = DIRECTION ( 'NONE',  ( 1.000000000000000000, -0.000000000000000000, -0.000000000000000000 ) ) ;
#15725 = FACE_BOUND ( 'NONE', #21938, .T. ) ;
#15726 = ORIENTED_EDGE ( 'NONE', *, *, #8894, .T. ) ;
#15727 = CARTESIAN_POINT ( 'NONE',  ( -281.2440776823446527, 269.1610889986682196, 150.0646579186752376 ) ) ;
#15728 = DIRECTION ( 'NONE',  ( 0.6964005597823107463, -0.7176533009294141507, 6.982962677686266711E-15 ) ) ;
#15729 = CONTEXT_DEPENDENT_SHAPE_REPRESENTATION ( #1958, #255 ) ;
#15730 = ORIENTED_EDGE ( 'NONE', *, *, #4782, .F. ) ;
#15731 = LINE ( 'NONE', #10181, #9259 ) ;
#15732 = VECTOR ( 'NONE', #14663, 1000.000000000000000 ) ;
#15733 = CARTESIAN_POINT ( 'NONE',  ( -280.4986342070537262, 269.7080393212556260, 146.1045205713626274 ) ) ;
#15734 = AXIS2_PLACEMENT_3D ( 'NONE', #8943, #11115, #19901 ) ;
#15735 = CARTESIAN_POINT ( 'NONE',  ( -107.6499999999999773, 30.00000000000001421, 0.000000000000000000 ) ) ;
#15736 = AXIS2_PLACEMENT_3D ( 'NONE', #7619, #15010, #20534 ) ;
#15737 = DIRECTION ( 'NONE',  ( 0.000000000000000000, 0.000000000000000000, 1.000000000000000000 ) ) ;
#15738 = ORIENTED_EDGE ( 'NONE', *, *, #3848, .F. ) ;
#15739 = DIRECTION ( 'NONE',  ( -1.000000000000000000, -0.000000000000000000, -0.000000000000000000 ) ) ;
#15741 = ORIENTED_EDGE ( 'NONE', *, *, #9883, .T. ) ;
#15740 = EDGE_LOOP ( 'NONE', ( #11525, #20697, #18980, #4899 ) ) ;
#15742 = CARTESIAN_POINT ( 'NONE',  ( -285.2000000000010118, 9.969634969241050884E-13, 0.000000000000000000 ) ) ;
#15743 = CARTESIAN_POINT ( 'NONE',  ( 7.500000000000000000, -1.645076096015019695, -7.030022527230891605 ) ) ;
#15744 = CARTESIAN_POINT ( 'NONE',  ( 65.00000000000001421, -56.79999999999939320, 125.0000000000002558 ) ) ;
#15745 = DIRECTION ( 'NONE',  ( 0.000000000000000000, 0.000000000000000000, -1.000000000000000000 ) ) ;
#15746 = DIRECTION ( 'NONE',  ( -1.000000000000000000, -0.000000000000000000, -0.000000000000000000 ) ) ;
#15747 = CARTESIAN_POINT ( 'NONE',  ( -280.0000000000000568, 269.9999999999999432, -144.9999999999999716 ) ) ;
#15748 = VECTOR ( 'NONE', #23566, 1000.000000000000000 ) ;
#15749 = VECTOR ( 'NONE', #10239, 1000.000000000000000 ) ;
#15750 = EDGE_LOOP ( 'NONE', ( #4579, #16693, #13530, #15721, #17036 ) ) ;
#15751 = AXIS2_PLACEMENT_3D ( 'NONE', #15896, #23469, #19366 ) ;
#15752 = CYLINDRICAL_SURFACE ( 'NONE', #5685, 5.249999999999942268 ) ;
#15753 = AXIS2_PLACEMENT_3D ( 'NONE', #10123, #17467, #13881 ) ;
#15754 = DIRECTION ( 'NONE',  ( 1.000000000000000000, 0.000000000000000000, -0.000000000000000000 ) ) ;
#15755 = DIRECTION ( 'NONE',  ( 0.000000000000000000, 0.000000000000000000, -1.000000000000000000 ) ) ;
#15756 = ADVANCED_FACE ( 'NONE', ( #10518 ), #7989, .F. ) ;
#15757 = EDGE_LOOP ( 'NONE', ( #14547, #20908, #14741, #5545 ) ) ;
#15758 = FACE_OUTER_BOUND ( 'NONE', #21278, .T. ) ;
#15759 = VERTEX_POINT ( 'NONE', #15366 ) ;
#15760 = FACE_OUTER_BOUND ( 'NONE', #9209, .T. ) ;
#15761 = CARTESIAN_POINT ( 'NONE',  ( -100.0000000000000000, -1400.000000000000000, 124.9999999999998295 ) ) ;
#15762 = ORIENTED_EDGE ( 'NONE', *, *, #20842, .T. ) ;
#15763 = CARTESIAN_POINT ( 'NONE',  ( 85.22886158240706322, 117.3074641843685129, -90.00000000000000000 ) ) ;
#15764 = DIRECTION ( 'NONE',  ( 0.000000000000000000, 0.000000000000000000, -1.000000000000000000 ) ) ;
#15765 = LINE ( 'NONE', #21422, #9182 ) ;
#15766 = PRODUCT ( 'MAS-186', 'MAS-186', '', ( #11476 ) ) ;
#15767 = EDGE_CURVE ( 'NONE', #14669, #15596, #16500, .T. ) ;
#15768 = TOROIDAL_SURFACE ( 'NONE', #14613, 6.500000000000000888, 1.500000000000000000 ) ;
#15769 = FACE_OUTER_BOUND ( 'NONE', #13982, .T. ) ;
#15770 = CIRCLE ( 'NONE', #333, 7.500000000000003553 ) ;
#15771 = CARTESIAN_POINT ( 'NONE',  ( 281.6578961534456766, 269.2533442688712171, 145.8089314698393366 ) ) ;
#15772 = LINE ( 'NONE', #1380, #5767 ) ;
#15773 = EDGE_CURVE ( 'NONE', #9508, #12526, #17230, .T. ) ;
#15774 = CIRCLE ( 'NONE', #21912, 2.055000000000001492 ) ;
#15775 = DIRECTION ( 'NONE',  ( 0.000000000000000000, 0.000000000000000000, 1.000000000000000000 ) ) ;
#15776 = ORIENTED_EDGE ( 'NONE', *, *, #2070, .F. ) ;
#15777 = SURFACE_STYLE_FILL_AREA ( #21318 ) ;
#15778 = DIRECTION ( 'NONE',  ( -1.000000000000000000, 0.000000000000000000, 0.000000000000000000 ) ) ;
#15779 = CARTESIAN_POINT ( 'NONE',  ( -4.000000000000000000, 0.8576368993457507139, -3.433240632782198709 ) ) ;
#15780 = EDGE_CURVE ( 'NONE', #14308, #8826, #4145, .T. ) ;
#15781 = VECTOR ( 'NONE', #12452, 1000.000000000000000 ) ;
#15782 = ORIENTED_EDGE ( 'NONE', *, *, #5427, .F. ) ;
#15783 = ORIENTED_EDGE ( 'NONE', *, *, #32, .F. ) ;
#15784 = DIRECTION ( 'NONE',  ( 0.000000000000000000, 0.000000000000000000, -1.000000000000000000 ) ) ;
#15785 = B_SPLINE_CURVE_WITH_KNOTS ( 'NONE', 3,
 ( #10700, #246, #9431, #11147, #7602, #13087, #22335, #22084, #19723, #11273 ),
 .UNSPECIFIED., .F., .F.,
 ( 4, 2, 2, 2, 4 ),
 ( 0.000000000000000000, 0.002305503304226489900, 0.004611006608452982401, 0.006916509912679474036, 0.009222013216905966537 ),
 .UNSPECIFIED. ) ;
#15786 = DIRECTION ( 'NONE',  ( -2.775557561562891351E-17, 1.000000000000000000, -0.000000000000000000 ) ) ;
#15787 = DIRECTION ( 'NONE',  ( 1.000000000000000000, 0.000000000000000000, 0.000000000000000000 ) ) ;
#15788 = AXIS2_PLACEMENT_3D ( 'NONE', #23229, #4884, #12292 ) ;
#15789 = STYLED_ITEM ( 'NONE', ( #6594 ), #6714 ) ;
#15790 = CARTESIAN_POINT ( 'NONE',  ( 131.8485914335931000, 81.49210221337234827, 28.34264858295340161 ) ) ;
#15791 = VECTOR ( 'NONE', #12566, 1000.000000000000000 ) ;
#15792 = DIRECTION ( 'NONE',  ( 1.000000000000000000, 0.000000000000000000, 0.000000000000000000 ) ) ;
#15793 = VECTOR ( 'NONE', #18643, 1000.000000000000000 ) ;
#15794 = CIRCLE ( 'NONE', #20789, 155.0000000000000284 ) ;
#15795 = LINE ( 'NONE', #13772, #1888 ) ;
#15796 = ORIENTED_EDGE ( 'NONE', *, *, #18749, .F. ) ;
#15797 = PLANE ( 'NONE',  #19481 ) ;
#15798 = CARTESIAN_POINT ( 'NONE',  ( -2.000000000000002665, -3.464101615137770374, -3.142992957459237680 ) ) ;
#15799 =( NAMED_UNIT ( * ) PLANE_ANGLE_UNIT ( ) SI_UNIT ( $, .RADIAN. ) );
#15800 = ORIENTED_EDGE ( 'NONE', *, *, #5579, .T. ) ;
#15801 = DIRECTION ( 'NONE',  ( 1.000000000000000000, -3.495664435217746987E-15, -0.000000000000000000 ) ) ;
#15802 = LINE ( 'NONE', #23621, #9167 ) ;
#15803 = CARTESIAN_POINT ( 'NONE',  ( -6.250000000000000000, -5.051814855409233473, -7.198902722707430257 ) ) ;
#15804 = VECTOR ( 'NONE', #7764, 1000.000000000000000 ) ;
#15805 = CARTESIAN_POINT ( 'NONE',  ( -23.72540896990115655, -1008.050072860352543, -145.0000000000001421 ) ) ;
#15806 = CARTESIAN_POINT ( 'NONE',  ( 2.500000000000002220, 2.357898499370434386, -3.469446951953614189E-15 ) ) ;
#15807 = CYLINDRICAL_SURFACE ( 'NONE', #14634, 2.649999999999999467 ) ;
#15808 = CARTESIAN_POINT ( 'NONE',  ( 2.500000000000002220, 2.357898499370434386, -3.469446951953614189E-15 ) ) ;
#15809 = ORIENTED_EDGE ( 'NONE', *, *, #15478, .F. ) ;
#15810 = ORIENTED_EDGE ( 'NONE', *, *, #9449, .F. ) ;
#15812 = VECTOR ( 'NONE', #3589, 1000.000000000000000 ) ;
#15811 = AXIS2_PLACEMENT_3D ( 'NONE', #21292, #8734, #21650 ) ;
#15813 = CARTESIAN_POINT ( 'NONE',  ( 0.000000000000000000, 0.000000000000000000, 0.000000000000000000 ) ) ;
#15814 = VECTOR ( 'NONE', #17786, 1000.000000000000114 ) ;
#15815 = CARTESIAN_POINT ( 'NONE',  ( 280.4974534559949007, 269.7094021484633117, 146.1021437883072167 ) ) ;
#15816 = EDGE_CURVE ( 'NONE', #3977, #321, #18959, .T. ) ;
#15817 = AXIS2_PLACEMENT_3D ( 'NONE', #20446, #20308, #7641 ) ;
#15818 = VECTOR ( 'NONE', #15695, 1000.000000000000000 ) ;
#15819 = VERTEX_POINT ( 'NONE', #19524 ) ;
#15820 = VECTOR ( 'NONE', #20688, 1000.000000000000000 ) ;
#15821 = AXIS2_PLACEMENT_3D ( 'NONE', #3685, #16637, #14716 ) ;
#15822 = EDGE_CURVE ( 'NONE', #1821, #15982, #23399, .T. ) ;
#15823 = DIRECTION ( 'NONE',  ( -1.000000000000000000, 0.000000000000000000, 0.000000000000000000 ) ) ;
#15824 = EDGE_LOOP ( 'NONE', ( #9263, #187, #123, #13424 ) ) ;
#15825 = FACE_OUTER_BOUND ( 'NONE', #402, .T. ) ;
#15826 = EDGE_CURVE ( 'NONE', #18385, #19431, #17645, .T. ) ;
#15827 = DIRECTION ( 'NONE',  ( 0.000000000000000000, 2.618450529776319755E-15, 1.000000000000000000 ) ) ;
#15828 = ORIENTED_EDGE ( 'NONE', *, *, #11719, .F. ) ;
#15829 = DIRECTION ( 'NONE',  ( -1.350636282998972974E-14, 0.000000000000000000, -1.000000000000000000 ) ) ;
#15830 = ADVANCED_FACE ( 'NONE', ( #10631, #8802, #2543, #9934, #17852, #17970, #8565 ), #14379, .F. ) ;
#15831 = ORIENTED_EDGE ( 'NONE', *, *, #8579, .T. ) ;
#15833 = TOROIDAL_SURFACE ( 'NONE', #13490, 2.700000000000000622, 0.2000000000000000111 ) ;
#15832 = AXIS2_PLACEMENT_3D ( 'NONE', #143, #16445, #14652 ) ;
#15834 = DIRECTION ( 'NONE',  ( 1.000000000000000000, 0.000000000000000000, 0.000000000000000000 ) ) ;
#15835 = COLOUR_RGB ( '',0.8941176470588234615, 0.8941176470588234615, 0.8941176470588234615 ) ;
#15837 = CIRCLE ( 'NONE', #18494, 5.249999999999949374 ) ;
#15836 = DIRECTION ( 'NONE',  ( 0.000000000000000000, 1.000000000000000000, 0.000000000000000000 ) ) ;
#15838 = ORIENTED_EDGE ( 'NONE', *, *, #18903, .F. ) ;
#15839 = ORIENTED_EDGE ( 'NONE', *, *, #1586, .F. ) ;
#15840 = FACE_OUTER_BOUND ( 'NONE', #11340, .T. ) ;
#15841 = CIRCLE ( 'NONE', #22373, 2.041999999999999815 ) ;
#15842 = AXIS2_PLACEMENT_3D ( 'NONE', #3543, #5027, #14557 ) ;
#15843 = CARTESIAN_POINT ( 'NONE',  ( -280.8700598572183935, 270.9755088701073191, -149.1320353020573464 ) ) ;
#15844 = CARTESIAN_POINT ( 'NONE',  ( -65.00000000000000000, -56.79999999999932925, 155.0000000000001705 ) ) ;
#15845 = DIRECTION ( 'NONE',  ( 0.000000000000000000, 0.000000000000000000, 1.000000000000000000 ) ) ;
#15846 = ORIENTED_EDGE ( 'NONE', *, *, #8275, .F. ) ;
#15847 = ADVANCED_FACE ( 'NONE', ( #17290, #4481 ), #11888, .T. ) ;
#15848 = DIRECTION ( 'NONE',  ( 0.000000000000000000, -1.000000000000000000, -4.694093751100962712E-16 ) ) ;
#15849 = EDGE_LOOP ( 'NONE', ( #5029, #9280, #5829, #12243 ) ) ;
#15850 = AXIS2_PLACEMENT_3D ( 'NONE', #12597, #8817, #14392 ) ;
#15851 = AXIS2_PLACEMENT_3D ( 'NONE', #6261, #12330, #21339 ) ;
#15852 = VECTOR ( 'NONE', #17795, 1000.000000000000000 ) ;
#15853 = ORIENTED_EDGE ( 'NONE', *, *, #21712, .T. ) ;
#15854 = CARTESIAN_POINT ( 'NONE',  ( -40.00000000000000000, 100.0000000000000000, 150.2000000000009550 ) ) ;
#15855 = ADVANCED_FACE ( 'NONE', ( #12347 ), #16642, .F. ) ;
#15856 = VERTEX_POINT ( 'NONE', #14835 ) ;
#15858 = ADVANCED_FACE ( 'NONE', ( #2004 ), #10698, .F. ) ;
#15857 = DIRECTION ( 'NONE',  ( -4.625929269271499719E-16, 0.000000000000000000, -1.000000000000000000 ) ) ;
#15859 = FACE_OUTER_BOUND ( 'NONE', #21335, .T. ) ;
#15860 = EDGE_LOOP ( 'NONE', ( #14160, #21204, #16794, #16131, #492 ) ) ;
#15861 = CARTESIAN_POINT ( 'NONE',  ( -281.3684637452626589, 268.4807971656550194, 150.1999999999999886 ) ) ;
#15862 = CARTESIAN_POINT ( 'NONE',  ( 5.560781378645573980, 6.809993116116507654E-16, -4.000000000000000000 ) ) ;
#15863 = ORIENTED_EDGE ( 'NONE', *, *, #2241, .T. ) ;
#15864 = CARTESIAN_POINT ( 'NONE',  ( 80.00000000000001421, -59.79999999999998295, 5.199999999999996625 ) ) ;
#15865 = DIRECTION ( 'NONE',  ( 0.000000000000000000, 0.000000000000000000, -1.000000000000000000 ) ) ;
#15866 = FACE_OUTER_BOUND ( 'NONE', #23264, .T. ) ;
#15867 = LINE ( 'NONE', #12509, #20767 ) ;
#15868 = VERTEX_POINT ( 'NONE', #11238 ) ;
#15869 = DIRECTION ( 'NONE',  ( -1.000000000000000000, -0.000000000000000000, -0.000000000000000000 ) ) ;
#15870 = PRODUCT_DEFINITION_SHAPE ( 'NONE', 'NONE',  #23834 ) ;
#15872 = ORIENTED_EDGE ( 'NONE', *, *, #17738, .F. ) ;
#15871 = ORIENTED_EDGE ( 'NONE', *, *, #1934, .T. ) ;
#15873 = EDGE_CURVE ( 'NONE', #6295, #7126, #18793, .T. ) ;
#15874 = CARTESIAN_POINT ( 'NONE',  ( 0.000000000000000000, -1.707388439385657340E-14, 145.0000000000000000 ) ) ;
#15875 = PLANE ( 'NONE',  #10447 ) ;
#15876 = DIRECTION ( 'NONE',  ( 1.000000000000000000, 0.000000000000000000, 0.000000000000000000 ) ) ;
#15877 = DIRECTION ( 'NONE',  ( 1.000000000000000000, 0.000000000000000000, 0.000000000000000000 ) ) ;
#15878 = CARTESIAN_POINT ( 'NONE',  ( 126.7787238282401745, 77.44864885511553609, -32.49999999999356959 ) ) ;
#15879 = B_SPLINE_CURVE_WITH_KNOTS ( 'NONE', 3,
 ( #19879, #20337, #5505, #3800, #16631, #18540 ),
 .UNSPECIFIED., .F., .F.,
 ( 4, 2, 4 ),
 ( -5.145455527297706927E-06, 0.0004153350442917282917, 0.0008358155441107560776 ),
 .UNSPECIFIED. ) ;
#15880 = CARTESIAN_POINT ( 'NONE',  ( -281.7592670532760053, 269.1520027839447948, -145.8708543776411659 ) ) ;
#15881 = EDGE_CURVE ( 'NONE', #1247, #5348, #9392, .T. ) ;
#15882 = EDGE_LOOP ( 'NONE', ( #20889, #23020 ) ) ;
#15883 =( REPRESENTATION_RELATIONSHIP ('NONE','NONE', #10127, #8987 ) REPRESENTATION_RELATIONSHIP_WITH_TRANSFORMATION ( #9099 )SHAPE_REPRESENTATION_RELATIONSHIP( ) );
#15884 = DIRECTION ( 'NONE',  ( 0.000000000000000000, 0.8660254037844380415, -0.5000000000000009992 ) ) ;
#15885 = EDGE_CURVE ( 'NONE', #22598, #10166, #10748, .T. ) ;
#15886 = ORIENTED_EDGE ( 'NONE', *, *, #22935, .T. ) ;
#15887 = DIRECTION ( 'NONE',  ( -0.3090169943749517811, 0.9510565162951520879, 0.000000000000000000 ) ) ;
#15888 = CARTESIAN_POINT ( 'NONE',  ( 24.33333333333333215, -89.99999999999998579, 0.000000000000000000 ) ) ;
#15889 = VERTEX_POINT ( 'NONE', #7563 ) ;
#15890 = DIRECTION ( 'NONE',  ( 0.000000000000000000, -0.000000000000000000, 1.000000000000000000 ) ) ;
#15891 = ORIENTED_EDGE ( 'NONE', *, *, #6638, .T. ) ;
#15892 = CARTESIAN_POINT ( 'NONE',  ( -79.99999999999995737, -62.00000000000001421, 5.199999999999997513 ) ) ;
#15893 = DIRECTION ( 'NONE',  ( -0.000000000000000000, -0.000000000000000000, 1.000000000000000000 ) ) ;
#15894 = ORIENTED_EDGE ( 'NONE', *, *, #23154, .F. ) ;
#15895 = PRESENTATION_STYLE_ASSIGNMENT (( #3177 ) ) ;
#15896 = CARTESIAN_POINT ( 'NONE',  ( 44.80746418436846312, -137.9031948627969655, -90.00000000000000000 ) ) ;
#15897 = CARTESIAN_POINT ( 'NONE',  ( 3.750000000000004441, -6.495190528383289141, 0.000000000000000000 ) ) ;
#15898 = LINE ( 'NONE', #23475, #12348 ) ;
#15899 = CARTESIAN_POINT ( 'NONE',  ( 0.000000000000000000, 2.357898499370433054, -1.951563910473907981E-15 ) ) ;
#15900 = DIRECTION ( 'NONE',  ( 0.000000000000000000, -3.495664435217746987E-15, -1.000000000000000000 ) ) ;
#15901 = ORIENTED_EDGE ( 'NONE', *, *, #3938, .F. ) ;
#15902 = CARTESIAN_POINT ( 'NONE',  ( -281.4928932188134354, -127.0000000000000568, -147.2000000000012960 ) ) ;
#15903 = DIRECTION ( 'NONE',  ( 0.000000000000000000, 1.000000000000000000, -1.471414886128461471E-15 ) ) ;
#15904 = ORIENTED_EDGE ( 'NONE', *, *, #8437, .T. ) ;
#15905 = EDGE_LOOP ( 'NONE', ( #18805, #9422, #4111, #11146 ) ) ;
#15906 = CARTESIAN_POINT ( 'NONE',  ( 0.000000000000000000, 1.865214261513747767E-15, -138.9999999999999716 ) ) ;
#15907 = CARTESIAN_POINT ( 'NONE',  ( -155.0000000000000284, 0.000000000000000000, 90.00000000000000000 ) ) ;
#15908 = EDGE_CURVE ( 'NONE', #18160, #3155, #6469, .T. ) ;
#15909 = ADVANCED_FACE ( 'NONE', ( #18092, #16293 ), #5169, .T. ) ;
#15910 = CARTESIAN_POINT ( 'NONE',  ( 131.6943452429968033, 81.74110354019241242, 28.74299381080684412 ) ) ;
#15911 = DIRECTION ( 'NONE',  ( -0.000000000000000000, -0.000000000000000000, -1.000000000000000000 ) ) ;
#15912 = LINE ( 'NONE', #23247, #17368 ) ;
#15913 = ORIENTED_EDGE ( 'NONE', *, *, #13058, .F. ) ;
#15914 = FACE_OUTER_BOUND ( 'NONE', #2521, .T. ) ;
#15915 = PLANE ( 'NONE',  #7271 ) ;
#15916 = EDGE_CURVE ( 'NONE', #15388, #3131, #16880, .T. ) ;
#15917 =( LENGTH_UNIT ( ) NAMED_UNIT ( * ) SI_UNIT ( .MILLI., .METRE. ) );
#15918 = ORIENTED_EDGE ( 'NONE', *, *, #8150, .F. ) ;
#15919 = CARTESIAN_POINT ( 'NONE',  ( 5.200000000000002842, 0.000000000000000000, 0.000000000000000000 ) ) ;
#15920 = FACE_OUTER_BOUND ( 'NONE', #21504, .T. ) ;
#15921 = CARTESIAN_POINT ( 'NONE',  ( 281.4928932188133217, -127.0000000000000568, 152.4000000000014268 ) ) ;
#15922 = CARTESIAN_POINT ( 'NONE',  ( 16.51661849037862950, -1018.838790234052340, -145.0000000000001137 ) ) ;
#15923 = FACE_OUTER_BOUND ( 'NONE', #21191, .T. ) ;
#15924 = DIRECTION ( 'NONE',  ( -0.000000000000000000, -0.000000000000000000, 1.000000000000000000 ) ) ;
#15925 = PLANE ( 'NONE',  #9366 ) ;
#15926 = VERTEX_POINT ( 'NONE', #3472 ) ;
#15927 = EDGE_LOOP ( 'NONE', ( #12083, #17884, #121, #519 ) ) ;
#15928 = CARTESIAN_POINT ( 'NONE',  ( -281.4301275412298651, 267.9452901038201844, -147.1999999999999602 ) ) ;
#15929 = CARTESIAN_POINT ( 'NONE',  ( -107.6499999999999773, -29.99999999999998579, 3.000000000000001332 ) ) ;
#15930 = ORIENTED_EDGE ( 'NONE', *, *, #17472, .T. ) ;
#15931 = DIRECTION ( 'NONE',  ( 0.000000000000000000, 0.000000000000000000, -1.000000000000000000 ) ) ;
#15932 = CARTESIAN_POINT ( 'NONE',  ( -2.999999999999996003, 21.50000000000000000, 0.000000000000000000 ) ) ;
#15933 = ORIENTED_EDGE ( 'NONE', *, *, #21375, .F. ) ;
#15934 = DIRECTION ( 'NONE',  ( 0.000000000000000000, 0.000000000000000000, 1.000000000000000000 ) ) ;
#15935 = ADVANCED_FACE ( 'NONE', ( #5283 ), #10880, .F. ) ;
#15936 = DIRECTION ( 'NONE',  ( -0.7071067811865383579, 8.659560562355047490E-17, -0.7071067811865567876 ) ) ;
#15937 = ORIENTED_EDGE ( 'NONE', *, *, #17298, .T. ) ;
#15938 = EDGE_CURVE ( 'NONE', #21406, #21409, #21881, .T. ) ;
#15939 = CARTESIAN_POINT ( 'NONE',  ( -134.8603954219446166, -1076.404761192049136, -31.65735141704661260 ) ) ;
#15940 = EDGE_LOOP ( 'NONE', ( #8998, #17031 ) ) ;
#15941 = PLANE ( 'NONE',  #12595 ) ;
#15942 = EDGE_CURVE ( 'NONE', #10771, #17172, #13853, .T. ) ;
#15943 = EDGE_CURVE ( 'NONE', #7205, #12818, #1847, .T. ) ;
#15944 = CARTESIAN_POINT ( 'NONE',  ( -7.914973979435149687, -3.817460047930451239, -7.907502498112421563 ) ) ;
#15945 = VERTEX_POINT ( 'NONE', #4424 ) ;
#15946 = ORIENTED_EDGE ( 'NONE', *, *, #5155, .T. ) ;
#15947 = LINE ( 'NONE', #14276, #4624 ) ;
#15948 = DIRECTION ( 'NONE',  ( 1.224646799147353207E-16, -2.002967142162725287E-32, -0.9999999999999998890 ) ) ;
#15949 = CARTESIAN_POINT ( 'NONE',  ( 2.712762565639649015, -3.052587955997662306, -3.430618716626630871 ) ) ;
#15950 = DIRECTION ( 'NONE',  ( 0.000000000000000000, 0.4999999999999991118, -0.8660254037844391517 ) ) ;
#15951 = CARTESIAN_POINT ( 'NONE',  ( 0.000000000000000000, 0.000000000000000000, 20.00000000000000000 ) ) ;
#15952 = EDGE_CURVE ( 'NONE', #5216, #10909, #5724, .T. ) ;
#15953 = VECTOR ( 'NONE', #14093, 1000.000000000000000 ) ;
#15954 = EDGE_LOOP ( 'NONE', ( #5083, #4813, #21852, #11027 ) ) ;
#15955 = CARTESIAN_POINT ( 'NONE',  ( 0.000000000000000000, 0.000000000000000000, 90.00000000000000000 ) ) ;
#15956 =( LENGTH_UNIT ( ) NAMED_UNIT ( * ) SI_UNIT ( .MILLI., .METRE. ) );
#15957 = CIRCLE ( 'NONE', #1662, 10.00000000000000000 ) ;
#15958 = VERTEX_POINT ( 'NONE', #17362 ) ;
#15959 = VERTEX_POINT ( 'NONE', #15314 ) ;
#15960 = CARTESIAN_POINT ( 'NONE',  ( 312.2000000000013529, -129.2000000000000455, -146.4928932188134070 ) ) ;
#15961 = ORIENTED_EDGE ( 'NONE', *, *, #994, .F. ) ;
#15962 = CARTESIAN_POINT ( 'NONE',  ( 0.000000000000000000, -2.357898499370432166, 3.035766082959412415E-15 ) ) ;
#15963 = AXIS2_PLACEMENT_3D ( 'NONE', #14871, #22205, #13579 ) ;
#15964 = ORIENTED_EDGE ( 'NONE', *, *, #23189, .T. ) ;
#15965 = PRODUCT_DEFINITION_SHAPE ( 'NONE', 'NONE',  #23808 ) ;
#15966 = CARTESIAN_POINT ( 'NONE',  ( -136.7463441837905975, -1072.975652424845066, 31.53022738271487313 ) ) ;
#15967 = DIRECTION ( 'NONE',  ( 8.144298233840332611E-17, 3.483493295888648978E-15, 1.000000000000000000 ) ) ;
#15968 = EDGE_CURVE ( 'NONE', #14720, #2646, #4558, .T. ) ;
#15969 = ORIENTED_EDGE ( 'NONE', *, *, #5152, .F. ) ;
#15970 = ADVANCED_FACE ( 'NONE', ( #17112 ), #22649, .F. ) ;
#15971 = DIRECTION ( 'NONE',  ( 1.000000000000000000, 0.000000000000000000, 0.000000000000000000 ) ) ;
#15972 = EDGE_CURVE ( 'NONE', #13509, #12504, #21527, .T. ) ;
#15973 = CARTESIAN_POINT ( 'NONE',  ( -280.8716261326570702, 269.1405375976307823, 146.7502846751313257 ) ) ;
#15974 = DIRECTION ( 'NONE',  ( 0.000000000000000000, -1.224646799147351975E-16, 1.000000000000000000 ) ) ;
#15975 = CARTESIAN_POINT ( 'NONE',  ( 124.4701338314433485, -1092.369831568443260, -27.49999999999351985 ) ) ;
#15976 = EDGE_CURVE ( 'NONE', #7122, #19888, #20482, .T. ) ;
#15977 = CARTESIAN_POINT ( 'NONE',  ( 0.000000000000000000, 0.000000000000000000, 90.00000000000000000 ) ) ;
#15978 = ORIENTED_EDGE ( 'NONE', *, *, #9386, .F. ) ;
#15979 = LINE ( 'NONE', #3029, #8460 ) ;
#15980 = EDGE_CURVE ( 'NONE', #6982, #19241, #2605, .T. ) ;
#15981 = CIRCLE ( 'NONE', #17896, 2.649999999999985700 ) ;
#15983 = ORIENTED_EDGE ( 'NONE', *, *, #107, .F. ) ;
#15982 = VERTEX_POINT ( 'NONE', #682 ) ;
#15984 = CARTESIAN_POINT ( 'NONE',  ( -44.99999999999998579, -64.79999999999941451, 340.0000000000002274 ) ) ;
#15985 = DIRECTION ( 'NONE',  ( 1.000000000000000000, 0.000000000000000000, -0.000000000000000000 ) ) ;
#15986 = DIRECTION ( 'NONE',  ( 0.000000000000000000, 0.000000000000000000, 1.000000000000000000 ) ) ;
#15987 = LINE ( 'NONE', #8615, #13939 ) ;
#15988 = LINE ( 'NONE', #19577, #11597 ) ;
#15989 = CARTESIAN_POINT ( 'NONE',  ( -93.00000000000000000, -79.73205080756885366, 3.000000000000002665 ) ) ;
#15990 = ORIENTED_EDGE ( 'NONE', *, *, #12076, .F. ) ;
#15991 = LINE ( 'NONE', #6322, #22775 ) ;
#15992 = VERTEX_POINT ( 'NONE', #20856 ) ;
#15993 = CARTESIAN_POINT ( 'NONE',  ( 60.00000000000000000, -135.7851947190609678, -3.814213562373143684 ) ) ;
#15994 = DIRECTION ( 'NONE',  ( 0.000000000000000000, 0.000000000000000000, 1.000000000000000000 ) ) ;
#15995 = CONTEXT_DEPENDENT_SHAPE_REPRESENTATION ( #22480, #7932 ) ;
#15996 = VERTEX_POINT ( 'NONE', #19019 ) ;
#15998 = CARTESIAN_POINT ( 'NONE',  ( -3.540020015735593439, -2.810662092924100630, -3.602146406945814672 ) ) ;
#15997 = VECTOR ( 'NONE', #5858, 999.9999999999998863 ) ;
#15999 = EDGE_LOOP ( 'NONE', ( #6909, #338 ) ) ;
#16000 = DIRECTION ( 'NONE',  ( 0.000000000000000000, 0.000000000000000000, 1.000000000000000000 ) ) ;
#16001 = CARTESIAN_POINT ( 'NONE',  ( -122.8605704798723224, 82.74225173005862644, 27.94500000000642359 ) ) ;
#16002 = ORIENTED_EDGE ( 'NONE', *, *, #5116, .F. ) ;
#16003 = SURFACE_STYLE_FILL_AREA ( #5014 ) ;
#16004 = SURFACE_SIDE_STYLE ('',( #14094 ) ) ;
#16005 = DIRECTION ( 'NONE',  ( -0.000000000000000000, 1.000000000000000000, 0.000000000000000000 ) ) ;
#16006 = CARTESIAN_POINT ( 'NONE',  ( 158.0000000000000568, -557.0000000000000000, 0.000000000000000000 ) ) ;
#16007 = EDGE_CURVE ( 'NONE', #6854, #3355, #17004, .T. ) ;
#16008 = DIRECTION ( 'NONE',  ( 0.000000000000000000, 0.000000000000000000, -1.000000000000000000 ) ) ;
#16009 = ADVANCED_FACE ( 'NONE', ( #9511 ), #23055, .F. ) ;
#16010 = DIRECTION ( 'NONE',  ( 0.000000000000000000, 0.000000000000000000, 1.000000000000000000 ) ) ;
#16011 = CARTESIAN_POINT ( 'NONE',  ( -146.0000000000005116, -494.4690652294800657, -29.99999999999356604 ) ) ;
#16012 = ORIENTED_EDGE ( 'NONE', *, *, #17099, .T. ) ;
#16013 =( LENGTH_UNIT ( ) NAMED_UNIT ( * ) SI_UNIT ( .MILLI., .METRE. ) );
#16014 = DIRECTION ( 'NONE',  ( 0.000000000000000000, 0.000000000000000000, -1.000000000000000000 ) ) ;
#16015 = DIRECTION ( 'NONE',  ( -0.8660254037844382635, 0.5000000000000005551, 0.000000000000000000 ) ) ;
#16016 = EDGE_LOOP ( 'NONE', ( #4632, #20014, #12048, #19682, #18650 ) ) ;
#16017 = APPLICATION_CONTEXT ( 'automotive_design' ) ;
#16018 = EDGE_LOOP ( 'NONE', ( #6155, #21813, #22451, #11983 ) ) ;
#16019 = VECTOR ( 'NONE', #6388, 1000.000000000000000 ) ;
#16020 = CARTESIAN_POINT ( 'NONE',  ( -93.00000000000000000, 3.053113317719180486E-13, 3.000000000000002665 ) ) ;
#16021 = CARTESIAN_POINT ( 'NONE',  ( 89.00000000000000000, -76.73205080756885366, 3.000000000000000000 ) ) ;
#16022 = CARTESIAN_POINT ( 'NONE',  ( -280.6807971656551217, 272.9999999999999432, 145.1244294735509470 ) ) ;
#16023 = AXIS2_PLACEMENT_3D ( 'NONE', #12502, #23668, #1799 ) ;
#16024 = LINE ( 'NONE', #20971, #17769 ) ;
#16025 = CARTESIAN_POINT ( 'NONE',  ( -283.1755088701073646, 271.9320353020571588, -145.6228333615949566 ) ) ;
#16026 = ORIENTED_EDGE ( 'NONE', *, *, #23530, .F. ) ;
#16027 = CARTESIAN_POINT ( 'NONE',  ( -69.99999999999997158, -87.33333333333338544, 124.9999999999999858 ) ) ;
#16028 = EDGE_LOOP ( 'NONE', ( #14385, #14032, #22801, #14162 ) ) ;
#16029 = CARTESIAN_POINT ( 'NONE',  ( 50.00000000000000000, -59.79999999999999716, 5.199999999999993960 ) ) ;
#16030 = PLANE ( 'NONE',  #8827 ) ;
#16031 = VECTOR ( 'NONE', #13893, 1000.000000000000000 ) ;
#16032 = LINE ( 'NONE', #23381, #22902 ) ;
#16033 = EDGE_LOOP ( 'NONE', ( #12875, #22450, #7981, #6099 ) ) ;
#16034 = DIRECTION ( 'NONE',  ( -1.000000000000000000, -2.775557561562891351E-17, 0.000000000000000000 ) ) ;
#16035 = CARTESIAN_POINT ( 'NONE',  ( 0.000000000000000000, -1000.000000000000000, 90.00000000000000000 ) ) ;
#16036 = PLANE ( 'NONE',  #11986 ) ;
#16037 = FACE_OUTER_BOUND ( 'NONE', #15497, .T. ) ;
#16038 = CYLINDRICAL_SURFACE ( 'NONE', #13869, 5.249999999999942268 ) ;
#16039 = PLANE ( 'NONE',  #20009 ) ;
#16040 = LINE ( 'NONE', #4563, #8227 ) ;
#16041 = AXIS2_PLACEMENT_3D ( 'NONE', #4580, #8326, #10274 ) ;
#16042 = CIRCLE ( 'NONE', #19829, 4.057500000000000107 ) ;
#16043 = ORIENTED_EDGE ( 'NONE', *, *, #4415, .F. ) ;
#16044 = ORIENTED_EDGE ( 'NONE', *, *, #12991, .T. ) ;
#16045 = LINE ( 'NONE', #23522, #9549 ) ;
#16046 = CARTESIAN_POINT ( 'NONE',  ( -144.8060344827586619, 7.497491405671214082, -2.775557561562891351E-14 ) ) ;
#16047 = ORIENTED_EDGE ( 'NONE', *, *, #3515, .T. ) ;
#16048 = FACE_OUTER_BOUND ( 'NONE', #18961, .T. ) ;
#16049 = CARTESIAN_POINT ( 'NONE',  ( -44.99999999999995026, -52.79999999999967031, 107.6500000000002046 ) ) ;
#16050 = AXIS2_PLACEMENT_3D ( 'NONE', #20110, #13190, #12909 ) ;
#16051 = ORIENTED_EDGE ( 'NONE', *, *, #13335, .F. ) ;
#16052 = DIRECTION ( 'NONE',  ( 1.000000000000000000, -7.709882115452476934E-17, 0.000000000000000000 ) ) ;
#16053 = CARTESIAN_POINT ( 'NONE',  ( 126.3653543294818178, 77.28387428943173632, -29.99999999999356604 ) ) ;
#16054 = AXIS2_PLACEMENT_3D ( 'NONE', #14749, #8959, #22079 ) ;
#16055 = VERTEX_POINT ( 'NONE', #11591 ) ;
#16056 = CARTESIAN_POINT ( 'NONE',  ( -135.1744136729190018, -1075.847854466910803, -32.17188107257633334 ) ) ;
#16057 = TOROIDAL_SURFACE ( 'NONE', #7534, 4.000000000000000000, 0.2500000000000000000 ) ;
#16058 = ORIENTED_EDGE ( 'NONE', *, *, #8667, .T. ) ;
#16059 =( REPRESENTATION_RELATIONSHIP ('NONE','NONE', #10127, #11474 ) REPRESENTATION_RELATIONSHIP_WITH_TRANSFORMATION ( #11300 )SHAPE_REPRESENTATION_RELATIONSHIP( ) );
#16060 = LINE ( 'NONE', #23758, #23268 ) ;
#16061 = ORIENTED_EDGE ( 'NONE', *, *, #580, .T. ) ;
#16062 = VERTEX_POINT ( 'NONE', #13654 ) ;
#16063 = EDGE_CURVE ( 'NONE', #11935, #15535, #22781, .T. ) ;
#16064 = DIRECTION ( 'NONE',  ( 0.000000000000000000, 2.618450529776313049E-15, 1.000000000000000000 ) ) ;
#16065 = PRODUCT_DEFINITION_SHAPE ( 'NONE', 'NONE',  #23850 ) ;
#16066 = CARTESIAN_POINT ( 'NONE',  ( -277.2000000000011255, -29.99999999999900879, -105.0000000000000142 ) ) ;
#16067 = CARTESIAN_POINT ( 'NONE',  ( -280.7154581756739162, 271.5968359015654983, -148.5570580646226801 ) ) ;
#16068 = AXIS2_PLACEMENT_3D ( 'NONE', #10200, #6436, #10457 ) ;
#16069 = CARTESIAN_POINT ( 'NONE',  ( -34.75000000000005684, 100.0000000000000000, 147.2000000000005855 ) ) ;
#16070 = DIRECTION ( 'NONE',  ( -1.000000000000000000, -0.000000000000000000, -0.000000000000000000 ) ) ;
#16071 = ADVANCED_FACE ( 'NONE', ( #5996 ), #22525, .F. ) ;
#16072 = VERTEX_POINT ( 'NONE', #20717 ) ;
#16073 = DIRECTION ( 'NONE',  ( -1.000000000000000000, 3.495664435217746987E-15, 0.000000000000000000 ) ) ;
#16074 = EDGE_CURVE ( 'NONE', #20963, #14990, #11343, .T. ) ;
#16075 = ADVANCED_FACE ( 'NONE', ( #22416 ), #7813, .F. ) ;
#16076 = EDGE_LOOP ( 'NONE', ( #22478, #8481, #21952, #618, #17634, #4655, #101, #22713 ) ) ;
#16077 = EDGE_CURVE ( 'NONE', #14252, #3378, #19587, .T. ) ;
#16078 = LINE ( 'NONE', #2667, #20237 ) ;
#16079 = DIRECTION ( 'NONE',  ( 1.000000000000000000, 0.000000000000000000, 0.000000000000000000 ) ) ;
#16080 = VERTEX_POINT ( 'NONE', #9755 ) ;
#16081 = VECTOR ( 'NONE', #4718, 1000.000000000000000 ) ;
#16082 = DIRECTION ( 'NONE',  ( 0.000000000000000000, -1.000000000000000000, 1.287488025362403787E-15 ) ) ;
#16083 = VERTEX_POINT ( 'NONE', #18653 ) ;
#16084 = DIRECTION ( 'NONE',  ( -1.000000000000000000, -0.000000000000000000, -0.000000000000000000 ) ) ;
#16085 = ORIENTED_EDGE ( 'NONE', *, *, #14395, .F. ) ;
#16086 = DIRECTION ( 'NONE',  ( -5.618537574013950123E-17, -3.483493295888648978E-15, -1.000000000000000000 ) ) ;
#16087 = CARTESIAN_POINT ( 'NONE',  ( 7.549006887134069643, -4.358421158401204032, -7.700127545397312367 ) ) ;
#16088 = TOROIDAL_SURFACE ( 'NONE', #22233, 5.384454397937118664, 0.5155456020628804703 ) ;
#16089 = DIRECTION ( 'NONE',  ( 0.000000000000000000, -0.7071067811865465735, 0.7071067811865485719 ) ) ;
#16090 = CARTESIAN_POINT ( 'NONE',  ( 1.680279846884594175E-14, -52.79999999999984794, 1.831306136874101946E-13 ) ) ;
#16091 = DIRECTION ( 'NONE',  ( 0.9423651898111409242, 0.3345860861306287903, -6.982962677686268288E-15 ) ) ;
#16092 = ORIENTED_EDGE ( 'NONE', *, *, #10682, .T. ) ;
#16093 = CARTESIAN_POINT ( 'NONE',  ( 5.200000000000002842, 3.306546357697854226E-16, 2.700000000000000622 ) ) ;
#16094 = CONICAL_SURFACE ( 'NONE', #4921, 2.055000000000001492, 0.7853981633974633780 ) ;
#16095 = EDGE_CURVE ( 'NONE', #17693, #1131, #11924, .T. ) ;
#16097 = ORIENTED_EDGE ( 'NONE', *, *, #9748, .F. ) ;
#16096 = ORIENTED_EDGE ( 'NONE', *, *, #15873, .T. ) ;
#16098 = DIRECTION ( 'NONE',  ( 1.000000000000000000, 0.000000000000000000, 6.123233995736766036E-17 ) ) ;
#16099 = DIRECTION ( 'NONE',  ( -0.000000000000000000, -0.000000000000000000, 1.000000000000000000 ) ) ;
#16100 = DIRECTION ( 'NONE',  ( -1.000000000000000000, -0.000000000000000000, -0.000000000000000000 ) ) ;
#16101 = EDGE_CURVE ( 'NONE', #17429, #22939, #11155, .T. ) ;
#16102 = DIRECTION ( 'NONE',  ( 1.000000000000000000, -3.495664435217746987E-15, -0.000000000000000000 ) ) ;
#16103 = EDGE_CURVE ( 'NONE', #18595, #9869, #1271, .T. ) ;
#16104 = CARTESIAN_POINT ( 'NONE',  ( 155.0000000000000284, -489.9999999999998863, 60.00000000000000000 ) ) ;
#16105 = ORIENTED_EDGE ( 'NONE', *, *, #11100, .T. ) ;
#16106 = FACE_BOUND ( 'NONE', #3724, .T. ) ;
#16107 = EDGE_CURVE ( 'NONE', #16906, #12117, #12706, .T. ) ;
#16108 = ORIENTED_EDGE ( 'NONE', *, *, #6766, .F. ) ;
#16109 = PRODUCT_DEFINITION ( 'UNKNOWN', '', #15075, #3716 ) ;
#16110 = VECTOR ( 'NONE', #22497, 1000.000000000000000 ) ;
#16111 = DIRECTION ( 'NONE',  ( 0.000000000000000000, 0.000000000000000000, 1.000000000000000000 ) ) ;
#16112 = CARTESIAN_POINT ( 'NONE',  ( 2.500000000000002220, -1.178949249685215417, 2.042000000000002036 ) ) ;
#16113 = VECTOR ( 'NONE', #22460, 1000.000000000000114 ) ;
#16114 = ORIENTED_EDGE ( 'NONE', *, *, #17271, .F. ) ;
#16115 = ORIENTED_EDGE ( 'NONE', *, *, #4460, .F. ) ;
#16116 = CARTESIAN_POINT ( 'NONE',  ( -129.3177328886526709, 85.45129583908980919, -29.83126738556711999 ) ) ;
#16117 = PLANE ( 'NONE',  #7949 ) ;
#16118 = ORIENTED_EDGE ( 'NONE', *, *, #22404, .T. ) ;
#16119 = CARTESIAN_POINT ( 'NONE',  ( -281.2439791848365758, 269.1488036478619961, 150.0335297745772039 ) ) ;
#16120 = CARTESIAN_POINT ( 'NONE',  ( 132.9260832389177267, 79.72254387118044860, 27.50000000000646239 ) ) ;
#16121 = DIRECTION ( 'NONE',  ( 0.000000000000000000, 0.000000000000000000, 1.000000000000000000 ) ) ;
#16122 = DIRECTION ( 'NONE',  ( -2.775557561562891351E-17, 1.000000000000000000, 4.694093751100962712E-16 ) ) ;
#16123 = DIRECTION ( 'NONE',  ( 0.000000000000000000, 0.000000000000000000, 1.000000000000000000 ) ) ;
#16124 = CARTESIAN_POINT ( 'NONE',  ( -288.2000000000006708, 90.00000000000102318, -35.00000000000001421 ) ) ;
#16125 = AXIS2_PLACEMENT_3D ( 'NONE', #4534, #12435, #11948 ) ;
#16126 = DIRECTION ( 'NONE',  ( 0.000000000000000000, 0.000000000000000000, 1.000000000000000000 ) ) ;
#16127 = EDGE_LOOP ( 'NONE', ( #19103, #9462, #18028, #3888 ) ) ;
#16128 = DIRECTION ( 'NONE',  ( 0.000000000000000000, 0.000000000000000000, -1.000000000000000000 ) ) ;
#16129 = CARTESIAN_POINT ( 'NONE',  ( -0.5276280594146446346, 4.314175951381965746, -3.320322319201721495 ) ) ;
#16130 = AXIS2_PLACEMENT_3D ( 'NONE', #18760, #20839, #20578 ) ;
#16131 = ORIENTED_EDGE ( 'NONE', *, *, #13822, .T. ) ;
#16132 = AXIS2_PLACEMENT_3D ( 'NONE', #3984, #11398, #18713 ) ;
#16133 = LINE ( 'NONE', #19377, #9613 ) ;
#16134 = CARTESIAN_POINT ( 'NONE',  ( 34.55500000000001393, 0.000000000000000000, 0.000000000000000000 ) ) ;
#16135 = DIRECTION ( 'NONE',  ( 0.000000000000000000, 0.000000000000000000, 1.000000000000000000 ) ) ;
#16136 = EDGE_CURVE ( 'NONE', #21370, #4511, #3007, .T. ) ;
#16137 = EDGE_CURVE ( 'NONE', #7824, #21414, #18433, .T. ) ;
#16138 = PLANE ( 'NONE',  #21839 ) ;
#16139 = EDGE_CURVE ( 'NONE', #19415, #11160, #19616, .T. ) ;
#16140 = DIRECTION ( 'NONE',  ( 0.000000000000000000, 1.177509268541832635E-16, -1.000000000000000000 ) ) ;
#16141 = EDGE_LOOP ( 'NONE', ( #16584, #478, #15276, #15133 ) ) ;
#16142 = FACE_BOUND ( 'NONE', #11399, .T. ) ;
#16143 = VERTEX_POINT ( 'NONE', #17695 ) ;
#16144 = CARTESIAN_POINT ( 'NONE',  ( 281.4928932188133217, -127.0000000000000568, 152.4000000000014268 ) ) ;
#16145 = LINE ( 'NONE', #12560, #18830 ) ;
#16146 = VECTOR ( 'NONE', #14411, 1000.000000000000000 ) ;
#16147 = SURFACE_STYLE_FILL_AREA ( #5267 ) ;
#16148 = AXIS2_PLACEMENT_3D ( 'NONE', #18223, #10652, #17990 ) ;
#16149 = ORIENTED_EDGE ( 'NONE', *, *, #3662, .F. ) ;
#16150 = CARTESIAN_POINT ( 'NONE',  ( -144.8060344827586619, 7.497491405671214082, 90.00000000000000000 ) ) ;
#16151 = DIRECTION ( 'NONE',  ( -0.000000000000000000, -0.000000000000000000, 1.000000000000000000 ) ) ;
#16152 = LINE ( 'NONE', #1868, #15419 ) ;
#16153 = CARTESIAN_POINT ( 'NONE',  ( 0.000000000000000000, 0.000000000000000000, -90.00000000000000000 ) ) ;
#16154 = DIRECTION ( 'NONE',  ( 0.000000000000000000, 0.4999999999999989453, -0.8660254037844393737 ) ) ;
#16155 = PLANE ( 'NONE',  #4972 ) ;
#16156 = CIRCLE ( 'NONE', #5351, 2.500000000000002220 ) ;
#16157 = CARTESIAN_POINT ( 'NONE',  ( 24.20041621714724300, 6.482064212728136710, 145.0000119999999697 ) ) ;
#16158 = ORIENTED_EDGE ( 'NONE', *, *, #10484, .T. ) ;
#16159 = ORIENTED_EDGE ( 'NONE', *, *, #21263, .F. ) ;
#16160 = DIRECTION ( 'NONE',  ( 0.000000000000000000, 0.000000000000000000, 1.000000000000000000 ) ) ;
#16161 = DIRECTION ( 'NONE',  ( 0.000000000000000000, -0.5000000000000009992, -0.8660254037844380415 ) ) ;
#16162 = VERTEX_POINT ( 'NONE', #19495 ) ;
#16163 = PRODUCT_DEFINITION_SHAPE ( 'NONE', 'NONE',  #23815 ) ;
#16164 = AXIS2_PLACEMENT_3D ( 'NONE', #3916, #11697, #9497 ) ;
#16165 = CARTESIAN_POINT ( 'NONE',  ( -7.497491405671719455, -144.8060344827586334, -2.775557561562891351E-14 ) ) ;
#16166 = DIRECTION ( 'NONE',  ( 1.000000000000000000, 0.000000000000000000, 0.000000000000000000 ) ) ;
#16168 = CIRCLE ( 'NONE', #23473, 5.199999999999982414 ) ;
#16167 = MECHANICAL_DESIGN_GEOMETRIC_PRESENTATION_REPRESENTATION (  '', ( #23524 ), #3423 ) ;
#16169 = VECTOR ( 'NONE', #19494, 1000.000000000000000 ) ;
#16170 = AXIS2_PLACEMENT_3D ( 'NONE', #3407, #23585, #21768 ) ;
#16171 = AXIS2_PLACEMENT_3D ( 'NONE', #11126, #1907, #17482 ) ;
#16172 = VERTEX_POINT ( 'NONE', #19378 ) ;
#16173 = CARTESIAN_POINT ( 'NONE',  ( -44.99999999999995026, -56.79999999999969873, 50.00000000000019895 ) ) ;
#16174 = AXIS2_PLACEMENT_3D ( 'NONE', #17893, #17787, #1347 ) ;
#16175 = CARTESIAN_POINT ( 'NONE',  ( 0.000000000000000000, 0.000000000000000000, 0.000000000000000000 ) ) ;
#16176 = ORIENTED_EDGE ( 'NONE', *, *, #7335, .F. ) ;
#16177 = ADVANCED_FACE ( 'NONE', ( #4542 ), #6352, .F. ) ;
#16178 = DIRECTION ( 'NONE',  ( 1.000000000000000000, 0.000000000000000000, -0.000000000000000000 ) ) ;
#16179 = AXIS2_PLACEMENT_3D ( 'NONE', #10492, #17827, #6963 ) ;
#16180 = ORIENTED_EDGE ( 'NONE', *, *, #2920, .T. ) ;
#16181 = EDGE_CURVE ( 'NONE', #2340, #218, #21137, .T. ) ;
#16182 = CARTESIAN_POINT ( 'NONE',  ( -45.24999999999996447, 100.0000000000000000, 150.2000000000009550 ) ) ;
#16183 = DIRECTION ( 'NONE',  ( -1.110223024625155594E-14, 0.000000000000000000, -1.000000000000000000 ) ) ;
#16184 = ORIENTED_EDGE ( 'NONE', *, *, #8587, .F. ) ;
#16185 = EDGE_LOOP ( 'NONE', ( #5578, #11969, #8291, #23063 ) ) ;
#16186 = CARTESIAN_POINT ( 'NONE',  ( -146.0000000000005116, -204.4690652294800657, -29.99999999999356604 ) ) ;
#16187 = CARTESIAN_POINT ( 'NONE',  ( -277.2000000000014097, -89.99999999999899103, -40.33333333333332860 ) ) ;
#16188 = AXIS2_PLACEMENT_3D ( 'NONE', #16351, #7160, #21886 ) ;
#16189 = FACE_BOUND ( 'NONE', #5541, .T. ) ;
#16190 = TOROIDAL_SURFACE ( 'NONE', #4986, 20.30000000000000071, 0.3000000000000059841 ) ;
#16191 = AXIS2_PLACEMENT_3D ( 'NONE', #16738, #20579, #14940 ) ;
#16193 = CARTESIAN_POINT ( 'NONE',  ( -146.4450000000001069, -784.4690652294805204, 27.50000000000642331 ) ) ;
#16192 = AXIS2_PLACEMENT_3D ( 'NONE', #12539, #23120, #19967 ) ;
#16194 = CIRCLE ( 'NONE', #18116, 10.00000000000000000 ) ;
#16195 = LINE ( 'NONE', #12239, #18594 ) ;
#16196 = AXIS2_PLACEMENT_3D ( 'NONE', #10998, #16871, #16519 ) ;
#16197 = ORIENTED_EDGE ( 'NONE', *, *, #11443, .F. ) ;
#16198 = DIRECTION ( 'NONE',  ( 1.302872740555339390E-32, -4.694093751100962712E-16, 1.000000000000000000 ) ) ;
#16199 = EDGE_LOOP ( 'NONE', ( #299, #14905, #12701, #22202 ) ) ;
#16200 = EDGE_CURVE ( 'NONE', #404, #22916, #10488, .T. ) ;
#16201 = FACE_OUTER_BOUND ( 'NONE', #3686, .T. ) ;
#16202 = EDGE_CURVE ( 'NONE', #21308, #11453, #10757, .T. ) ;
#16203 = CYLINDRICAL_SURFACE ( 'NONE', #13404, 2.649999999999999467 ) ;
#16205 = CIRCLE ( 'NONE', #10046, 2.500000000000000888 ) ;
#16204 = AXIS2_PLACEMENT_3D ( 'NONE', #3902, #9245, #3771 ) ;
#16206 = VERTEX_POINT ( 'NONE', #16021 ) ;
#16207 = CARTESIAN_POINT ( 'NONE',  ( 0.000000000000000000, -4.685197434473811207, 4.770489558936219510E-15 ) ) ;
#16208 = VECTOR ( 'NONE', #14187, 1000.000000000000000 ) ;
#16209 = VECTOR ( 'NONE', #15486, 1000.000000000000114 ) ;
#16210 = VECTOR ( 'NONE', #17600, 999.9999999999998863 ) ;
#16211 = ORIENTED_EDGE ( 'NONE', *, *, #10545, .T. ) ;
#16212 = B_SPLINE_CURVE_WITH_KNOTS ( 'NONE', 3,
 ( #12834, #8812, #3586, #19904, #8691, #9048 ),
 .UNSPECIFIED., .F., .F.,
 ( 4, 2, 4 ),
 ( -3.640115492410698714E-06, 0.0002066546034006521879, 0.0004169493222937151081 ),
 .UNSPECIFIED. ) ;
#16213 = CYLINDRICAL_SURFACE ( 'NONE', #2874, 7.500000000000007105 ) ;
#16214 = EDGE_CURVE ( 'NONE', #1996, #9003, #19742, .T. ) ;
#16215 = ORIENTED_EDGE ( 'NONE', *, *, #11100, .F. ) ;
#16216 = LINE ( 'NONE', #16324, #10053 ) ;
#16217 = CARTESIAN_POINT ( 'NONE',  ( -280.4357197208658476, 269.7771302778488689, 145.9755403010747159 ) ) ;
#16218 = EDGE_CURVE ( 'NONE', #8135, #5418, #23367, .T. ) ;
#16219 = CARTESIAN_POINT ( 'NONE',  ( 89.00000000000000000, -79.73205080756883945, 2.999999999999988898 ) ) ;
#16220 = CARTESIAN_POINT ( 'NONE',  ( 2.500000000000000000, 1.178949249685218525, 2.041999999999999371 ) ) ;
#16221 = CARTESIAN_POINT ( 'NONE',  ( 40.00000000000000000, 100.0000000000000000, 150.2000000000009550 ) ) ;
#16222 = ADVANCED_BREP_SHAPE_REPRESENTATION ( '', ( #4076, #11210 ), #16951 ) ;
#16223 = EDGE_LOOP ( 'NONE', ( #2233, #7076, #21105, #15286 ) ) ;
#16224 = PRODUCT_DEFINITION_FORMATION_WITH_SPECIFIED_SOURCE ( 'ANY', '', #5359, .NOT_KNOWN. ) ;
#16225 = CARTESIAN_POINT ( 'NONE',  ( -7.500000000000001776, 0.000000000000000000, 0.000000000000000000 ) ) ;
#16226 = COLOUR_RGB ( '',0.8941176470588234615, 0.8941176470588234615, 0.8941176470588234615 ) ;
#16227 = VECTOR ( 'NONE', #14137, 1000.000000000000000 ) ;
#16228 = AXIS2_PLACEMENT_3D ( 'NONE', #17839, #4918, #10504 ) ;
#16230 = ORIENTED_EDGE ( 'NONE', *, *, #21440, .F. ) ;
#16229 = VERTEX_POINT ( 'NONE', #6471 ) ;
#16231 = DIRECTION ( 'NONE',  ( 0.000000000000000000, 0.000000000000000000, -1.000000000000000000 ) ) ;
#16232 = CYLINDRICAL_SURFACE ( 'NONE', #16598, 7.500000000000007105 ) ;
#16233 = FACE_OUTER_BOUND ( 'NONE', #14235, .T. ) ;
#16234 = ORIENTED_EDGE ( 'NONE', *, *, #18170, .T. ) ;
#16235 = CARTESIAN_POINT ( 'NONE',  ( 146.4449999999997374, -209.9999999999996874, 32.50000000000641620 ) ) ;
#16236 = ORIENTED_EDGE ( 'NONE', *, *, #4761, .T. ) ;
#16237 = CARTESIAN_POINT ( 'NONE',  ( 105.0000000000000000, 35.00000000000000000, 3.000000000000001332 ) ) ;
#16238 = ORIENTED_EDGE ( 'NONE', *, *, #2636, .T. ) ;
#16239 = ADVANCED_FACE ( 'NONE', ( #10232 ), #1022, .F. ) ;
#16240 = VERTEX_POINT ( 'NONE', #20093 ) ;
#16241 = EDGE_CURVE ( 'NONE', #5068, #506, #16897, .T. ) ;
#16242 = PLANE ( 'NONE',  #8837 ) ;
#16243 = DIRECTION ( 'NONE',  ( -0.9423651898111408132, -0.3345860861306287348, 6.982962677686266711E-15 ) ) ;
#16244 = VERTEX_POINT ( 'NONE', #17941 ) ;
#16245 = ORIENTED_EDGE ( 'NONE', *, *, #9180, .F. ) ;
#16246 = DIRECTION ( 'NONE',  ( -0.000000000000000000, -0.000000000000000000, -1.000000000000000000 ) ) ;
#16247 = ORIENTED_EDGE ( 'NONE', *, *, #4135, .T. ) ;
#16248 = CARTESIAN_POINT ( 'NONE',  ( 2.500000000000000000, 1.768423874527822903, -1.021000000000002350 ) ) ;
#16249 = ADVANCED_FACE ( 'NONE', ( #6602 ), #21084, .F. ) ;
#16250 = CARTESIAN_POINT ( 'NONE',  ( 133.4121500950858490, 78.90641005980415912, 32.24990070396069086 ) ) ;
#16251 = DIRECTION ( 'NONE',  ( -1.000000000000000000, 0.000000000000000000, 0.000000000000000000 ) ) ;
#16252 = ADVANCED_FACE ( 'NONE', ( #12190 ), #19265, .F. ) ;
#16253 = DIRECTION ( 'NONE',  ( -1.000000000000000000, -0.000000000000000000, -0.000000000000000000 ) ) ;
#16254 = DIRECTION ( 'NONE',  ( 0.000000000000000000, -0.8660254037844390407, -0.4999999999999992784 ) ) ;
#16255 = DIRECTION ( 'NONE',  ( 0.000000000000000000, 0.000000000000000000, 1.000000000000000000 ) ) ;
#16256 = VERTEX_POINT ( 'NONE', #21212 ) ;
#16257 =( NAMED_UNIT ( * ) SI_UNIT ( $, .STERADIAN. ) SOLID_ANGLE_UNIT ( ) );
#16258 = CARTESIAN_POINT ( 'NONE',  ( 79.04925354955338435, -121.5574576620390843, -90.00000000000000000 ) ) ;
#16259 = CARTESIAN_POINT ( 'NONE',  ( -2.807080416178626692, 3.225969019225154444, -3.502507215260441065 ) ) ;
#16260 = ORIENTED_EDGE ( 'NONE', *, *, #21474, .T. ) ;
#16261 = FACE_OUTER_BOUND ( 'NONE', #1600, .T. ) ;
#16262 = CARTESIAN_POINT ( 'NONE',  ( 8.673617379884035472E-16, 4.618802153517012954, 0.000000000000000000 ) ) ;
#16264 = CARTESIAN_POINT ( 'NONE',  ( -285.0938770989753834, 269.1689414351989740, 146.2440776823445105 ) ) ;
#16263 = PRODUCT_DEFINITION_SHAPE ( 'NONE', 'NONE',  #23845 ) ;
#16265 = CARTESIAN_POINT ( 'NONE',  ( 145.9999999999997726, -801.0618695410399823, 32.05500000000641592 ) ) ;
#16266 = CARTESIAN_POINT ( 'NONE',  ( -146.0000000000005684, -786.5240652294799020, -29.99999999999356604 ) ) ;
#16267 = ORIENTED_EDGE ( 'NONE', *, *, #6601, .F. ) ;
#16268 = DIRECTION ( 'NONE',  ( -1.000000000000000000, 0.000000000000000000, -0.000000000000000000 ) ) ;
#16269 = ORIENTED_EDGE ( 'NONE', *, *, #18498, .F. ) ;
#16270 = DIRECTION ( 'NONE',  ( 1.000000000000000000, -0.000000000000000000, -0.000000000000000000 ) ) ;
#16271 = DIRECTION ( 'NONE',  ( -1.000000000000000000, -0.000000000000000000, 0.000000000000000000 ) ) ;
#16272 = EDGE_CURVE ( 'NONE', #23723, #6529, #18807, .T. ) ;
#16273 = CARTESIAN_POINT ( 'NONE',  ( 137.9031948627967950, 44.80746418436894629, -90.00000000000000000 ) ) ;
#16274 = EDGE_CURVE ( 'NONE', #22960, #18604, #10958, .T. ) ;
#16275 = VERTEX_POINT ( 'NONE', #23604 ) ;
#16276 = CARTESIAN_POINT ( 'NONE',  ( -67.34999999999996589, -112.6666666666667140, 0.000000000000000000 ) ) ;
#16277 = CARTESIAN_POINT ( 'NONE',  ( 146.0000000000002558, -801.0618695410406644, -32.05499999999356930 ) ) ;
#16278 = ADVANCED_FACE ( 'NONE', ( #1732, #14562 ), #9123, .F. ) ;
#16279 = CARTESIAN_POINT ( 'NONE',  ( 0.000000000000000000, 0.000000000000000000, -0.3080913168122742518 ) ) ;
#16280 = FACE_BOUND ( 'NONE', #11710, .T. ) ;
#16281 = ADVANCED_FACE ( 'NONE', ( #12663 ), #15475, .F. ) ;
#16282 = DIRECTION ( 'NONE',  ( -0.8090169943749507819, 0.5877852522924686962, 0.000000000000000000 ) ) ;
#16283 = DIRECTION ( 'NONE',  ( -0.000000000000000000, 0.4999999999999979461, -0.8660254037844397068 ) ) ;
#16284 = LINE ( 'NONE', #7083, #6684 ) ;
#16285 = VERTEX_POINT ( 'NONE', #1849 ) ;
#16286 = ADVANCED_FACE ( 'NONE', ( #7419 ), #8772, .F. ) ;
#16287 = EDGE_LOOP ( 'NONE', ( #17430, #7332, #13233, #4810, #7108 ) ) ;
#16288 = CARTESIAN_POINT ( 'NONE',  ( 60.00000000000000000, -131.7994082814339833, 3.000000000000000000 ) ) ;
#16289 = CARTESIAN_POINT ( 'NONE',  ( 2.500000000000000000, 0.000000000000000000, 0.000000000000000000 ) ) ;
#16290 = ADVANCED_FACE ( 'NONE', ( #12901 ), #23491, .F. ) ;
#16291 = VERTEX_POINT ( 'NONE', #7302 ) ;
#16292 = DIRECTION ( 'NONE',  ( -0.000000000000000000, 1.000000000000000000, -3.469446951953613794E-15 ) ) ;
#16293 = FACE_OUTER_BOUND ( 'NONE', #1840, .T. ) ;
#16294 = ORIENTED_EDGE ( 'NONE', *, *, #11892, .F. ) ;
#16295 = DIRECTION ( 'NONE',  ( -0.000000000000000000, -0.000000000000000000, 1.000000000000000000 ) ) ;
#16296 = DIRECTION ( 'NONE',  ( -1.000000000000000000, 0.000000000000000000, 0.000000000000000000 ) ) ;
#16297 = ORIENTED_EDGE ( 'NONE', *, *, #310, .F. ) ;
#16298 = LINE ( 'NONE', #23642, #23320 ) ;
#16299 = VERTEX_POINT ( 'NONE', #13015 ) ;
#16300 = EDGE_CURVE ( 'NONE', #21414, #7824, #7164, .T. ) ;
#16301 = DIRECTION ( 'NONE',  ( 1.000000000000000000, 0.000000000000000000, 0.000000000000000000 ) ) ;
#16302 = DIRECTION ( 'NONE',  ( 0.000000000000000000, 0.000000000000000000, -1.000000000000000000 ) ) ;
#16303 = ORIENTED_EDGE ( 'NONE', *, *, #713, .F. ) ;
#16304 = ORIENTED_EDGE ( 'NONE', *, *, #2023, .F. ) ;
#16305 = CARTESIAN_POINT ( 'NONE',  ( 285.1999999999999318, 268.4807971656551331, -146.3684637452624315 ) ) ;
#16306 = AXIS2_PLACEMENT_3D ( 'NONE', #11466, #13770, #21089 ) ;
#16307 = DIRECTION ( 'NONE',  ( 6.123233995736766036E-17, 0.000000000000000000, 1.000000000000000000 ) ) ;
#16308 = CARTESIAN_POINT ( 'NONE',  ( -127.7157292285630632, 87.82777678213136596, -32.48402282453940870 ) ) ;
#16309 = CARTESIAN_POINT ( 'NONE',  ( -42.98333333333330586, -89.99999999999997158, 3.000000000000000000 ) ) ;
#16310 = DIRECTION ( 'NONE',  ( 3.202566417187928841E-16, -1.000000000000000000, 3.469446951953614583E-15 ) ) ;
#16311 = VERTEX_POINT ( 'NONE', #21789 ) ;
#16312 = EDGE_CURVE ( 'NONE', #22518, #1647, #5258, .T. ) ;
#16313 = DIRECTION ( 'NONE',  ( -2.220299922379604070E-16, -1.000000000000000000, 0.000000000000000000 ) ) ;
#16314 = SURFACE_STYLE_FILL_AREA ( #451 ) ;
#16315 = EDGE_CURVE ( 'NONE', #15889, #1686, #16366, .T. ) ;
#16316 = AXIS2_PLACEMENT_3D ( 'NONE', #12013, #6521, #19422 ) ;
#16317 = DIRECTION ( 'NONE',  ( -1.110223024625157172E-14, 0.000000000000000000, -1.000000000000000000 ) ) ;
#16318 = DIRECTION ( 'NONE',  ( 0.000000000000000000, 0.000000000000000000, -1.000000000000000000 ) ) ;
#16319 = EDGE_LOOP ( 'NONE', ( #12450, #7068, #11426, #15370 ) ) ;
#16320 = CARTESIAN_POINT ( 'NONE',  ( -117.3074641843675749, 85.22886158240835641, -90.00000000000000000 ) ) ;
#16321 = ORIENTED_EDGE ( 'NONE', *, *, #7703, .F. ) ;
#16322 = LINE ( 'NONE', #21851, #6355 ) ;
#16323 = ORIENTED_EDGE ( 'NONE', *, *, #15368, .T. ) ;
#16324 = CARTESIAN_POINT ( 'NONE',  ( -288.2000000000006708, 90.00000000000102318, -37.64999999999999147 ) ) ;
#16325 = PRESENTATION_STYLE_ASSIGNMENT (( #13092 ) ) ;
#16326 = DIRECTION ( 'NONE',  ( -0.000000000000000000, -0.000000000000000000, 1.000000000000000000 ) ) ;
#16327 = CIRCLE ( 'NONE', #21337, 4.000000000000000000 ) ;
#16328 =( REPRESENTATION_RELATIONSHIP ('NONE','NONE', #10127, #14711 ) REPRESENTATION_RELATIONSHIP_WITH_TRANSFORMATION ( #11929 )SHAPE_REPRESENTATION_RELATIONSHIP( ) );
#16329 = CARTESIAN_POINT ( 'NONE',  ( -44.99999999999995026, -52.79999999999969873, 50.00000000000018474 ) ) ;
#16330 = CARTESIAN_POINT ( 'NONE',  ( -7.499999999999999112, -2.930060224340425901, -0.4701183149080249146 ) ) ;
#16331 = ORIENTED_EDGE ( 'NONE', *, *, #10710, .T. ) ;
#16332 = DIRECTION ( 'NONE',  ( 0.000000000000000000, 1.224646799147353207E-16, 1.000000000000000000 ) ) ;
#16334 = ORIENTED_EDGE ( 'NONE', *, *, #23025, .T. ) ;
#16333 = EDGE_LOOP ( 'NONE', ( #4463, #4622 ) ) ;
#16335 = DIRECTION ( 'NONE',  ( 1.000000000000000000, 0.000000000000000000, 0.000000000000000000 ) ) ;
#16336 = CARTESIAN_POINT ( 'NONE',  ( 67.35000000000002274, -112.6666666666666714, 3.000000000000000000 ) ) ;
#16337 = DIRECTION ( 'NONE',  ( 0.000000000000000000, 0.000000000000000000, -1.000000000000000000 ) ) ;
#16338 = ORIENTED_EDGE ( 'NONE', *, *, #6633, .F. ) ;
#16339 = AXIS2_PLACEMENT_3D ( 'NONE', #7787, #659, #4152 ) ;
#16340 = LINE ( 'NONE', #12763, #21442 ) ;
#16341 = CIRCLE ( 'NONE', #5148, 7.500000000000000888 ) ;
#16342 = DIRECTION ( 'NONE',  ( -1.000000000000000000, 1.408839003528726857E-14, 6.982962677686266711E-15 ) ) ;
#16343 = EDGE_LOOP ( 'NONE', ( #6649, #599, #20946, #14892 ) ) ;
#16344 = DIRECTION ( 'NONE',  ( 0.9423651898111409242, 0.3345860861306287903, -6.982962677686268288E-15 ) ) ;
#16345 = FACE_OUTER_BOUND ( 'NONE', #16016, .T. ) ;
#16346 = ORIENTED_EDGE ( 'NONE', *, *, #4696, .F. ) ;
#16347 = ORIENTED_EDGE ( 'NONE', *, *, #21109, .F. ) ;
#16348 = LINE ( 'NONE', #18506, #10272 ) ;
#16349 = ORIENTED_EDGE ( 'NONE', *, *, #17522, .F. ) ;
#16350 = DIRECTION ( 'NONE',  ( -0.000000000000000000, 1.000000000000000000, -3.469446951953613794E-15 ) ) ;
#16351 = CARTESIAN_POINT ( 'NONE',  ( 137.9031948627967950, 44.80746418436894629, 90.00000000000000000 ) ) ;
#16352 = CARTESIAN_POINT ( 'NONE',  ( 2.805705207896068476, -3.226868319750173075, -3.503898532754370354 ) ) ;
#16353 = AXIS2_PLACEMENT_3D ( 'NONE', #14149, #21125, #19308 ) ;
#16354 = DIRECTION ( 'NONE',  ( 0.000000000000000000, -1.000000000000000000, 0.000000000000000000 ) ) ;
#16355 = DIRECTION ( 'NONE',  ( -1.110223024625157172E-14, 0.000000000000000000, -1.000000000000000000 ) ) ;
#16356 =( LENGTH_UNIT ( ) NAMED_UNIT ( * ) SI_UNIT ( .MILLI., .METRE. ) );
#16357 = EDGE_LOOP ( 'NONE', ( #14732, #18398, #13567, #13689 ) ) ;
#16358 = EDGE_CURVE ( 'NONE', #15253, #23038, #14533, .T. ) ;
#16359 = SURFACE_STYLE_USAGE ( .BOTH. , #8531 ) ;
#16360 = CARTESIAN_POINT ( 'NONE',  ( 7.497491405671719455, -144.8060344827586334, -90.00000000000000000 ) ) ;
#16361 = DIRECTION ( 'NONE',  ( 1.000000000000000000, -0.000000000000000000, -0.000000000000000000 ) ) ;
#16362 = EDGE_CURVE ( 'NONE', #4214, #10971, #3689, .T. ) ;
#16363 = EDGE_CURVE ( 'NONE', #2548, #1247, #5255, .T. ) ;
#16364 = EDGE_LOOP ( 'NONE', ( #14957, #15116, #7036, #14242 ) ) ;
#16365 = DIRECTION ( 'NONE',  ( 0.000000000000000000, 0.000000000000000000, 1.000000000000000000 ) ) ;
#16366 = LINE ( 'NONE', #10849, #1393 ) ;
#16367 = EDGE_CURVE ( 'NONE', #11975, #1617, #19863, .T. ) ;
#16368 = CARTESIAN_POINT ( 'NONE',  ( -282.2000000000010687, -19.99999999999898392, 105.0000000000000000 ) ) ;
#16369 = VECTOR ( 'NONE', #11725, 1000.000000000000000 ) ;
#16370 = AXIS2_PLACEMENT_3D ( 'NONE', #9587, #419, #16949 ) ;
#16371 = DIRECTION ( 'NONE',  ( 0.000000000000000000, 0.000000000000000000, 1.000000000000000000 ) ) ;
#16372 = CARTESIAN_POINT ( 'NONE',  ( 280.6846668451111668, 271.7159870726002850, -148.4379565153279259 ) ) ;
#16373 = VECTOR ( 'NONE', #18777, 1000.000000000000000 ) ;
#16374 = ORIENTED_EDGE ( 'NONE', *, *, #16218, .T. ) ;
#16375 = PLANE ( 'NONE',  #10815 ) ;
#16376 = ORIENTED_EDGE ( 'NONE', *, *, #23770, .T. ) ;
#16377 = DIRECTION ( 'NONE',  ( -1.000000000000000000, 0.000000000000000000, 0.000000000000000000 ) ) ;
#16378 = CARTESIAN_POINT ( 'NONE',  ( 155.0000000000000284, -489.9999999999998863, 60.00000000000000000 ) ) ;
#16379 = ORIENTED_EDGE ( 'NONE', *, *, #15916, .F. ) ;
#16380 = CARTESIAN_POINT ( 'NONE',  ( 123.1031131805784469, -1094.184009126531237, -31.11320915316581193 ) ) ;
#16381 = CARTESIAN_POINT ( 'NONE',  ( -117.3074641843669781, -85.22886158240918064, -90.00000000000000000 ) ) ;
#16382 = FACE_OUTER_BOUND ( 'NONE', #9273, .T. ) ;
#16383 = PLANE ( 'NONE',  #15395 ) ;
#16384 = CARTESIAN_POINT ( 'NONE',  ( 89.00000000000000000, -152.9999999999996874, 129.9038105676659711 ) ) ;
#16385 = CARTESIAN_POINT ( 'NONE',  ( 8.055391459054625614, 23.72315261474502890, 145.0000119999999981 ) ) ;
#16386 = ORIENTED_EDGE ( 'NONE', *, *, #21802, .T. ) ;
#16387 = CIRCLE ( 'NONE', #18618, 35.00000000000000711 ) ;
#16388 = VERTEX_POINT ( 'NONE', #69 ) ;
#16389 = CARTESIAN_POINT ( 'NONE',  ( -7.500000000000000000, -4.330127018922198090, -10.00000000000000000 ) ) ;
#16390 = LINE ( 'NONE', #14475, #5793 ) ;
#16391 = ORIENTED_EDGE ( 'NONE', *, *, #17170, .F. ) ;
#16392 = ADVANCED_FACE ( 'NONE', ( #3312 ), #1508, .T. ) ;
#16393 = AXIS2_PLACEMENT_3D ( 'NONE', #9878, #15787, #17235 ) ;
#16394 = DIRECTION ( 'NONE',  ( 1.000000000000000000, 0.000000000000000000, 0.000000000000000000 ) ) ;
#16395 = CARTESIAN_POINT ( 'NONE',  ( 4.599534470797546959, -6.460478697736932396, -7.590212325761396706 ) ) ;
#16396 = EDGE_CURVE ( 'NONE', #18250, #644, #20657, .T. ) ;
#16397 = ORIENTED_EDGE ( 'NONE', *, *, #9505, .T. ) ;
#16398 = CARTESIAN_POINT ( 'NONE',  ( 280.1244266708878285, 269.9999999999999432, 145.2880230824754904 ) ) ;
#16399 = EDGE_CURVE ( 'NONE', #493, #12317, #3547, .T. ) ;
#16400 = DIRECTION ( 'NONE',  ( -0.7071067811865320296, 9.875400524328840493E-15, 0.7071067811865631159 ) ) ;
#16401 = ORIENTED_EDGE ( 'NONE', *, *, #8447, .T. ) ;
#16402 = CONICAL_SURFACE ( 'NONE', #6383, 2.055000000000001492, 0.7853981633974633780 ) ;
#16403 = DIRECTION ( 'NONE',  ( -1.350636282998972974E-14, 0.000000000000000000, -1.000000000000000000 ) ) ;
#16404 = CARTESIAN_POINT ( 'NONE',  ( 2.500000000000000000, 0.000000000000000000, 0.000000000000000000 ) ) ;
#16405 = EDGE_CURVE ( 'NONE', #4707, #23406, #20271, .T. ) ;
#16406 = AXIS2_PLACEMENT_3D ( 'NONE', #12586, #19896, #3348 ) ;
#16407 = ORIENTED_EDGE ( 'NONE', *, *, #17298, .F. ) ;
#16408 = CARTESIAN_POINT ( 'NONE',  ( 7.703928834700305650, 4.447865386531936416, -7.917997657324733929 ) ) ;
#16410 = CARTESIAN_POINT ( 'NONE',  ( 7.497491405671719455, -144.8060344827586334, -2.775557561562891351E-14 ) ) ;
#16409 = PRODUCT_DEFINITION ( 'UNKNOWN', '', #20823, #11017 ) ;
#16411 = EDGE_CURVE ( 'NONE', #4336, #5418, #14157, .T. ) ;
#16412 = DIRECTION ( 'NONE',  ( 0.000000000000000000, 0.000000000000000000, -1.000000000000000000 ) ) ;
#16413 = ORIENTED_EDGE ( 'NONE', *, *, #13936, .T. ) ;
#16414 = VERTEX_POINT ( 'NONE', #22615 ) ;
#16415 = CARTESIAN_POINT ( 'NONE',  ( 285.0938770989752697, 269.1689414351989740, -146.2440776823444537 ) ) ;
#16416 = VECTOR ( 'NONE', #17398, 1000.000000000000000 ) ;
#16417 = SHAPE_DEFINITION_REPRESENTATION ( #1879, #21947 ) ;
#16418 = CARTESIAN_POINT ( 'NONE',  ( -127.5319552722386760, 88.09441757049788180, -27.57920702976963767 ) ) ;
#16419 = CARTESIAN_POINT ( 'NONE',  ( 2.699999999999997513, 0.000000000000000000, -19.99999999999998934 ) ) ;
#16420 = ORIENTED_EDGE ( 'NONE', *, *, #16533, .T. ) ;
#16421 = CARTESIAN_POINT ( 'NONE',  ( 1.636246173744688726, -24.99999999999999289, 145.0000119999999697 ) ) ;
#16422 = AXIS2_PLACEMENT_3D ( 'NONE', #2785, #19807, #3257 ) ;
#16423 = AXIS2_PLACEMENT_3D ( 'NONE', #13860, #20944, #3294 ) ;
#16424 = CARTESIAN_POINT ( 'NONE',  ( 0.000000000000000000, 2.357898499370431722, -2.818925648462311528E-15 ) ) ;
#16425 = FACE_OUTER_BOUND ( 'NONE', #15905, .T. ) ;
#16426 = ORIENTED_EDGE ( 'NONE', *, *, #3202, .F. ) ;
#16427 = CARTESIAN_POINT ( 'NONE',  ( 2.621328321948289020, 7.606199919103058704, -7.633618187056857352 ) ) ;
#16428 = ORIENTED_EDGE ( 'NONE', *, *, #2518, .T. ) ;
#16429 = ADVANCED_FACE ( 'NONE', ( #9599 ), #6080, .F. ) ;
#16430 = EDGE_CURVE ( 'NONE', #8654, #14664, #15285, .T. ) ;
#16431 = VECTOR ( 'NONE', #18874, 1000.000000000000000 ) ;
#16432 = FACE_OUTER_BOUND ( 'NONE', #5704, .T. ) ;
#16433 = EDGE_CURVE ( 'NONE', #19823, #15352, #11318, .T. ) ;
#16434 = CARTESIAN_POINT ( 'NONE',  ( -1.390230914382372118, -4.043987460488664532, -3.502507215260523665 ) ) ;
#16435 = ORIENTED_EDGE ( 'NONE', *, *, #3197, .F. ) ;
#16436 = CARTESIAN_POINT ( 'NONE',  ( 0.3198814748697593746, 4.434118497892183264, -0.3507732604232499107 ) ) ;
#16437 = CARTESIAN_POINT ( 'NONE',  ( -21.69578997558838296, -1012.528766853774982, 145.0000119999999697 ) ) ;
#16438 = CARTESIAN_POINT ( 'NONE',  ( 0.000000000000000000, 0.000000000000000000, 90.00000000000000000 ) ) ;
#16439 = CARTESIAN_POINT ( 'NONE',  ( -69.99999999999997158, -87.33333333333338544, 148.0000000000000000 ) ) ;
#16440 = CARTESIAN_POINT ( 'NONE',  ( -24.99999999999996092, -37.41657386773943728, 169.9999999999999716 ) ) ;
#16441 = ORIENTED_EDGE ( 'NONE', *, *, #16827, .T. ) ;
#16442 = DIRECTION ( 'NONE',  ( -2.775557561562891351E-17, 1.000000000000000000, -0.000000000000000000 ) ) ;
#16444 = EDGE_LOOP ( 'NONE', ( #3981, #10206, #6651, #5612 ) ) ;
#16443 = ORIENTED_EDGE ( 'NONE', *, *, #7058, .T. ) ;
#16445 = DIRECTION ( 'NONE',  ( 1.224646799147353207E-16, -4.064521778635712183E-50, -1.000000000000000000 ) ) ;
#16446 = CARTESIAN_POINT ( 'NONE',  ( -2.500000000000000888, 0.000000000000000000, -4.974599999999998801 ) ) ;
#16447 = CIRCLE ( 'NONE', #11871, 2.500000000000000444 ) ;
#16448 = CARTESIAN_POINT ( 'NONE',  ( 0.2727178028658734932, 0.000000000000000000, 0.000000000000000000 ) ) ;
#16449 = B_SPLINE_CURVE_WITH_KNOTS ( 'NONE', 3,
 ( #17591, #1041, #15803, #17956, #5271, #6975, #18408, #11087, #7320 ),
 .UNSPECIFIED., .F., .F.,
 ( 4, 2, 1, 2, 4 ),
 ( 0.000000000000000000, 0.002165063509461097064, 0.004330127018922194128, 0.006495190528383290758, 0.008660254037844389990 ),
 .UNSPECIFIED. ) ;
#16450 = EDGE_LOOP ( 'NONE', ( #13620, #1787, #8682, #2565 ) ) ;
#16451 = DIRECTION ( 'NONE',  ( -0.000000000000000000, -0.000000000000000000, 1.000000000000000000 ) ) ;
#16452 = DIRECTION ( 'NONE',  ( 1.000000000000000000, 0.000000000000000000, 0.000000000000000000 ) ) ;
#16453 = VERTEX_POINT ( 'NONE', #4139 ) ;
#16454 = B_SPLINE_CURVE_WITH_KNOTS ( 'NONE', 3,
 ( #6727, #6842, #1283, #21453, #21229 ),
 .UNSPECIFIED., .F., .F.,
 ( 4, 1, 4 ),
 ( 0.000000000000000000, 0.002309401076758505790, 0.004618802153517011580 ),
 .UNSPECIFIED. ) ;
#16455 = CARTESIAN_POINT ( 'NONE',  ( 30.00000000000000000, 2.516649172247811061E-16, -2.055000000000006821 ) ) ;
#16456 = DIRECTION ( 'NONE',  ( -1.000000000000000000, -0.000000000000000000, -0.000000000000000000 ) ) ;
#16457 = CIRCLE ( 'NONE', #23773, 7.500000000000000000 ) ;
#16458 = CONTEXT_DEPENDENT_SHAPE_REPRESENTATION ( #21437, #19312 ) ;
#16459 = ORIENTED_EDGE ( 'NONE', *, *, #14055, .T. ) ;
#16460 = ORIENTED_EDGE ( 'NONE', *, *, #11860, .F. ) ;
#16461 = CARTESIAN_POINT ( 'NONE',  ( -100.0000000000000000, -1420.000000000000000, 124.9999999999998295 ) ) ;
#16462 = EDGE_LOOP ( 'NONE', ( #8486, #2961, #13298, #1305, #1944, #5956, #7781 ) ) ;
#16463 = CIRCLE ( 'NONE', #277, 2.499999999999998668 ) ;
#16464 = CARTESIAN_POINT ( 'NONE',  ( -129.2813770747755484, 85.50638651248962674, 29.34395718620176297 ) ) ;
#16465 = CYLINDRICAL_SURFACE ( 'NONE', #1510, 2.649999999999985700 ) ;
#16466 = CARTESIAN_POINT ( 'NONE',  ( 144.8060344827585482, 7.497491405673235576, -2.775557561562891351E-14 ) ) ;
#16467 = LINE ( 'NONE', #19686, #4187 ) ;
#16468 = DIRECTION ( 'NONE',  ( 1.000000000000000000, 0.000000000000000000, 0.000000000000000000 ) ) ;
#16469 = EDGE_LOOP ( 'NONE', ( #15344, #15170, #4897 ) ) ;
#16470 = CARTESIAN_POINT ( 'NONE',  ( 0.000000000000000000, -1000.000000000000000, 0.000000000000000000 ) ) ;
#16471 = CARTESIAN_POINT ( 'NONE',  ( -20.00000000000000000, 2.449293598294706513E-15, -150.0000000000000000 ) ) ;
#16472 = CARTESIAN_POINT ( 'NONE',  ( -37.68333333333335844, -89.99999999999997158, 0.000000000000000000 ) ) ;
#16473 = ORIENTED_EDGE ( 'NONE', *, *, #23317, .F. ) ;
#16474 = FACE_OUTER_BOUND ( 'NONE', #17210, .T. ) ;
#16475 = DIRECTION ( 'NONE',  ( -1.000000000000000000, 0.000000000000000000, 0.000000000000000000 ) ) ;
#16476 = VECTOR ( 'NONE', #7901, 1000.000000000000000 ) ;
#16477 = CIRCLE ( 'NONE', #21863, 145.0000000000000284 ) ;
#16478 = EDGE_CURVE ( 'NONE', #9321, #11736, #2912, .T. ) ;
#16479 = CARTESIAN_POINT ( 'NONE',  ( -285.2000000000000455, 267.7999999999999545, 146.4928932188134354 ) ) ;
#16480 = DIRECTION ( 'NONE',  ( 0.9510565162951534202, 0.3090169943749478398, 0.000000000000000000 ) ) ;
#16481 = DIRECTION ( 'NONE',  ( 0.000000000000000000, 0.000000000000000000, 1.000000000000000000 ) ) ;
#16482 = ORIENTED_EDGE ( 'NONE', *, *, #17441, .F. ) ;
#16483 = DIRECTION ( 'NONE',  ( 1.000000000000000000, 0.000000000000000000, 0.000000000000000000 ) ) ;
#16484 = EDGE_LOOP ( 'NONE', ( #20588, #5497, #19689, #9349 ) ) ;
#16485 = EDGE_CURVE ( 'NONE', #8982, #22322, #22386, .T. ) ;
#16486 = DIRECTION ( 'NONE',  ( 1.000000000000000000, 0.000000000000000000, 0.000000000000000000 ) ) ;
#16487 = DIRECTION ( 'NONE',  ( 0.000000000000000000, 0.000000000000000000, -1.000000000000000000 ) ) ;
#16488 = ADVANCED_FACE ( 'NONE', ( #13500, #20819, #5726 ), #18626, .F. ) ;
#16489 = ORIENTED_EDGE ( 'NONE', *, *, #1940, .T. ) ;
#16490 = CIRCLE ( 'NONE', #3752, 5.249999999999991118 ) ;
#16491 = CARTESIAN_POINT ( 'NONE',  ( 124.3711180590059229, -1092.503257236082163, -32.49999999999351985 ) ) ;
#16492 = CARTESIAN_POINT ( 'NONE',  ( -281.4928932188135491, 5.173457871231061435E-13, 150.2000000000009550 ) ) ;
#16493 = DIRECTION ( 'NONE',  ( -0.7232617928448825673, 0.6905739489807055653, 6.982962677686266711E-15 ) ) ;
#16495 = AXIS2_PLACEMENT_3D ( 'NONE', #13598, #4365, #14894 ) ;
#16494 = CARTESIAN_POINT ( 'NONE',  ( -282.2000000000013529, -89.99999999999897682, 24.33333333333333215 ) ) ;
#16496 = EDGE_CURVE ( 'NONE', #13908, #23165, #9482, .T. ) ;
#16497 = DIRECTION ( 'NONE',  ( 1.000000000000000000, 0.000000000000000000, 0.000000000000000000 ) ) ;
#16498 = VECTOR ( 'NONE', #7674, 1000.000000000000000 ) ;
#16499 = CARTESIAN_POINT ( 'NONE',  ( -6.482064212728111841, 24.20041621714724656, 145.0000119999999697 ) ) ;
#16500 = CIRCLE ( 'NONE', #17288, 20.00000000000001776 ) ;
#16501 = VERTEX_POINT ( 'NONE', #4389 ) ;
#16502 = ORIENTED_EDGE ( 'NONE', *, *, #19732, .F. ) ;
#16503 = CYLINDRICAL_SURFACE ( 'NONE', #21112, 2.500000000000002220 ) ;
#16505 = CARTESIAN_POINT ( 'NONE',  ( 0.2500000000000002220, 0.000000000000000000, 4.250000000000000000 ) ) ;
#16504 =( REPRESENTATION_RELATIONSHIP ('NONE','NONE', #10127, #18083 ) REPRESENTATION_RELATIONSHIP_WITH_TRANSFORMATION ( #6219 )SHAPE_REPRESENTATION_RELATIONSHIP( ) );
#16506 = ORIENTED_EDGE ( 'NONE', *, *, #6400, .T. ) ;
#16507 = CARTESIAN_POINT ( 'NONE',  ( -280.0000000000000568, 267.7999999999999545, -146.4928932188134354 ) ) ;
#16508 = CARTESIAN_POINT ( 'NONE',  ( 7.169303301815196150, -4.521054846639319003, -7.349897473155491134 ) ) ;
#16509 = CIRCLE ( 'NONE', #19575, 2.100000000000000089 ) ;
#16510 = ORIENTED_EDGE ( 'NONE', *, *, #3928, .T. ) ;
#16511 = CARTESIAN_POINT ( 'NONE',  ( 280.9952621458755289, 268.9079617568158938, 146.9223300543793584 ) ) ;
#16512 = DIRECTION ( 'NONE',  ( 0.5000000000000005551, -0.8660254037844383745, 0.000000000000000000 ) ) ;
#16513 = ORIENTED_EDGE ( 'NONE', *, *, #12377, .T. ) ;
#16514 = AXIS2_PLACEMENT_3D ( 'NONE', #12395, #14305, #29 ) ;
#16515 = AXIS2_PLACEMENT_3D ( 'NONE', #5774, #20597, #13290 ) ;
#16516 = FACE_OUTER_BOUND ( 'NONE', #17518, .T. ) ;
#16517 = DIRECTION ( 'NONE',  ( -1.000000000000000000, 0.000000000000000000, 0.000000000000000000 ) ) ;
#16518 = VECTOR ( 'NONE', #14551, 1000.000000000000000 ) ;
#16519 = DIRECTION ( 'NONE',  ( 0.000000000000000000, 1.000000000000000000, -4.183096374613631247E-18 ) ) ;
#16520 = ORIENTED_EDGE ( 'NONE', *, *, #13287, .T. ) ;
#16521 = EDGE_CURVE ( 'NONE', #7507, #11951, #17989, .T. ) ;
#16522 = LINE ( 'NONE', #9401, #2599 ) ;
#16523 = CARTESIAN_POINT ( 'NONE',  ( -136.6968504244148335, -1073.068359172759074, 31.65640384616915526 ) ) ;
#16524 = DIRECTION ( 'NONE',  ( 1.000000000000000000, -0.000000000000000000, -0.000000000000000000 ) ) ;
#16525 = ORIENTED_EDGE ( 'NONE', *, *, #5930, .T. ) ;
#16526 = EDGE_LOOP ( 'NONE', ( #9734, #627, #15137 ) ) ;
#16527 = DIRECTION ( 'NONE',  ( 1.000000000000000000, -3.495664435217746987E-15, -0.000000000000000000 ) ) ;
#16528 = APPLICATION_PROTOCOL_DEFINITION ( 'draft international standard', 'automotive_design', 1998, #20475 ) ;
#16529 = CARTESIAN_POINT ( 'NONE',  ( -126.7581711459445160, 89.20411804604358963, -31.53250949154612925 ) ) ;
#16530 = ADVANCED_FACE ( 'NONE', ( #13372 ), #11681, .T. ) ;
#16531 = DIRECTION ( 'NONE',  ( 0.000000000000000000, 2.618450529776326854E-15, 1.000000000000000000 ) ) ;
#16532 = FACE_BOUND ( 'NONE', #22565, .T. ) ;
#16533 = EDGE_CURVE ( 'NONE', #21142, #20571, #1979, .T. ) ;
#16534 = CIRCLE ( 'NONE', #16908, 2.649999999999992806 ) ;
#16535 = ORIENTED_EDGE ( 'NONE', *, *, #20348, .F. ) ;
#16536 = CIRCLE ( 'NONE', #19603, 2.055000000000001492 ) ;
#16537 = CARTESIAN_POINT ( 'NONE',  ( -1.636246173744679178, -24.99999999999999645, 145.0000119999999697 ) ) ;
#16538 = VECTOR ( 'NONE', #1289, 1000.000000000000000 ) ;
#16539 = AXIS2_PLACEMENT_3D ( 'NONE', #21392, #23568, #6786 ) ;
#16540 = ADVANCED_FACE ( 'NONE', ( #652 ), #3315, .T. ) ;
#16541 = ADVANCED_FACE ( 'NONE', ( #8021 ), #8634, .F. ) ;
#16542 = CIRCLE ( 'NONE', #15006, 7.500000000000000000 ) ;
#16543 = DIRECTION ( 'NONE',  ( 3.736327486719275871E-16, -1.000000000000000000, 3.469446951953614189E-15 ) ) ;
#16544 = DIRECTION ( 'NONE',  ( -0.000000000000000000, 0.4999999999999979461, -0.8660254037844397068 ) ) ;
#16545 = ORIENTED_EDGE ( 'NONE', *, *, #2804, .T. ) ;
#16546 = LINE ( 'NONE', #14514, #14507 ) ;
#16547 = ORIENTED_EDGE ( 'NONE', *, *, #11925, .F. ) ;
#16548 = PRODUCT_DEFINITION_SHAPE ( 'NONE', 'NONE',  #11555 ) ;
#16549 = AXIS2_PLACEMENT_3D ( 'NONE', #9740, #15300, #9618 ) ;
#16551 = AXIS2_PLACEMENT_3D ( 'NONE', #9113, #16468, #11191 ) ;
#16550 = STYLED_ITEM ( 'NONE', ( #12542 ), #20508 ) ;
#16553 = CARTESIAN_POINT ( 'NONE',  ( -51.87806360044816500, 135.4018704341555974, 90.00000000000000000 ) ) ;
#16552 = CIRCLE ( 'NONE', #6145, 145.0000000000000284 ) ;
#16554 = LINE ( 'NONE', #1132, #3255 ) ;
#16555 = ORIENTED_EDGE ( 'NONE', *, *, #23209, .F. ) ;
#16556 = CARTESIAN_POINT ( 'NONE',  ( 0.000000000000000000, 0.000000000000000000, 150.0000000000000284 ) ) ;
#16557 = AXIS2_PLACEMENT_3D ( 'NONE', #17061, #2555, #18848 ) ;
#16558 = VECTOR ( 'NONE', #18784, 1000.000000000000000 ) ;
#16559 = CARTESIAN_POINT ( 'NONE',  ( -69.99999999999997158, -112.6666666666667140, 144.9999999999999716 ) ) ;
#16560 = ADVANCED_FACE ( 'NONE', ( #8153 ), #19501, .F. ) ;
#16561 = CARTESIAN_POINT ( 'NONE',  ( -24.99999999999998224, -1000.000000000000000, 145.0000059999999280 ) ) ;
#16562 = FACE_OUTER_BOUND ( 'NONE', #14404, .T. ) ;
#16563 = CARTESIAN_POINT ( 'NONE',  ( 125.9168667295997892, -1090.387741168242883, -29.34624901867154634 ) ) ;
#16564 = PLANE ( 'NONE',  #11633 ) ;
#16565 = ORIENTED_EDGE ( 'NONE', *, *, #3241, .F. ) ;
#16566 = EDGE_CURVE ( 'NONE', #17543, #18148, #22979, .T. ) ;
#16567 = CYLINDRICAL_SURFACE ( 'NONE', #4537, 160.0000000000000000 ) ;
#16568 = CYLINDRICAL_SURFACE ( 'NONE', #21856, 23.50000000000000000 ) ;
#16569 = FILL_AREA_STYLE_COLOUR ( '', #4968 ) ;
#16570 = EDGE_CURVE ( 'NONE', #19928, #22176, #19125, .T. ) ;
#16572 = ORIENTED_EDGE ( 'NONE', *, *, #20620, .F. ) ;
#16571 = ORIENTED_EDGE ( 'NONE', *, *, #9791, .T. ) ;
#16573 = DIRECTION ( 'NONE',  ( 1.000000000000000000, 0.000000000000000000, 0.000000000000000000 ) ) ;
#16574 = EDGE_CURVE ( 'NONE', #9060, #2405, #4996, .T. ) ;
#16576 = CIRCLE ( 'NONE', #6157, 2.649999999999971934 ) ;
#16575 = AXIS2_PLACEMENT_3D ( 'NONE', #16470, #64, #21892 ) ;
#16577 = LINE ( 'NONE', #12758, #22732 ) ;
#16578 = CARTESIAN_POINT ( 'NONE',  ( 281.3684637452625452, 268.4807971656550762, -150.1999999999999318 ) ) ;
#16579 = EDGE_CURVE ( 'NONE', #13966, #7277, #17798, .T. ) ;
#16580 =( GEOMETRIC_REPRESENTATION_CONTEXT ( 3 ) GLOBAL_UNCERTAINTY_ASSIGNED_CONTEXT ( ( #17123 ) ) GLOBAL_UNIT_ASSIGNED_CONTEXT ( ( #8606, #21514, #19704 ) ) REPRESENTATION_CONTEXT ( 'NONE', 'WORKASPACE' ) );
#16581 = AXIS2_PLACEMENT_3D ( 'NONE', #2089, #2204, #6079 ) ;
#16582 = CONICAL_SURFACE ( 'NONE', #19655, 2.055000000000000160, 0.7853981633974639331 ) ;
#16583 = VECTOR ( 'NONE', #1877, 1000.000000000000000 ) ;
#16584 = ORIENTED_EDGE ( 'NONE', *, *, #23556, .F. ) ;
#16585 = CARTESIAN_POINT ( 'NONE',  ( 0.000000000000000000, 0.000000000000000000, -150.0000000000000000 ) ) ;
#16586 = ORIENTED_EDGE ( 'NONE', *, *, #20698, .T. ) ;
#16587 = CARTESIAN_POINT ( 'NONE',  ( 45.00000000000002132, -56.79999999999933635, 195.0000000000002274 ) ) ;
#16588 = VERTEX_POINT ( 'NONE', #15989 ) ;
#16589 = CYLINDRICAL_SURFACE ( 'NONE', #18853, 5.249999999999942268 ) ;
#16590 = DIRECTION ( 'NONE',  ( 0.000000000000000000, -0.5000000000000011102, -0.8660254037844379305 ) ) ;
#16591 = CONTEXT_DEPENDENT_SHAPE_REPRESENTATION ( #20987, #8144 ) ;
#16592 = ORIENTED_EDGE ( 'NONE', *, *, #3534, .T. ) ;
#16593 = CARTESIAN_POINT ( 'NONE',  ( 124.8644691973863701, -1091.836575763269366, 27.56549073392524818 ) ) ;
#16594 = AXIS2_PLACEMENT_3D ( 'NONE', #16066, #23178, #1432 ) ;
#16595 = EDGE_LOOP ( 'NONE', ( #8032, #5528, #8589, #14936 ) ) ;
#16596 = LINE ( 'NONE', #5708, #20953 ) ;
#16597 = PRESENTATION_LAYER_ASSIGNMENT (  '', '', ( #3790 ) ) ;
#16598 = AXIS2_PLACEMENT_3D ( 'NONE', #1595, #10808, #19943 ) ;
#16599 = CARTESIAN_POINT ( 'NONE',  ( 134.0610795706241447, 77.79865694966419198, 30.80845853161018155 ) ) ;
#16600 = CIRCLE ( 'NONE', #18512, 145.0000000000000284 ) ;
#16601 = VECTOR ( 'NONE', #22247, 1000.000000000000000 ) ;
#16602 = CARTESIAN_POINT ( 'NONE',  ( 4.211140560182196957, -2.431303136016555122, -3.745885042887436622 ) ) ;
#16603 = ADVANCED_FACE ( 'NONE', ( #19112 ), #21297, .F. ) ;
#16604 = PLANE ( 'NONE',  #17899 ) ;
#16605 = CARTESIAN_POINT ( 'NONE',  ( -45.00000000000000000, 272.9999999999999432, -5.249999999999991118 ) ) ;
#16606 = ORIENTED_EDGE ( 'NONE', *, *, #20124, .T. ) ;
#16607 = PRESENTATION_STYLE_ASSIGNMENT (( #20201 ) ) ;
#16608 = EDGE_CURVE ( 'NONE', #12879, #3080, #2916, .T. ) ;
#16609 = CARTESIAN_POINT ( 'NONE',  ( -7.500000000000001776, 2.932633423934442263, -0.4709827563909292358 ) ) ;
#16610 = CARTESIAN_POINT ( 'NONE',  ( -20.63749999999999929, 0.000000000000000000, 0.000000000000000000 ) ) ;
#16611 = ADVANCED_FACE ( 'NONE', ( #21404 ), #771, .F. ) ;
#16612 = ORIENTED_EDGE ( 'NONE', *, *, #20627, .F. ) ;
#16613 = EDGE_CURVE ( 'NONE', #15333, #15682, #11919, .T. ) ;
#16614 = DIRECTION ( 'NONE',  ( 1.000000000000000000, 0.000000000000000000, 0.000000000000000000 ) ) ;
#16615 = DIRECTION ( 'NONE',  ( 1.000000000000000000, -0.000000000000000000, 6.982962677686266711E-15 ) ) ;
#16616 = VECTOR ( 'NONE', #14158, 1000.000000000000000 ) ;
#16617 = AXIS2_PLACEMENT_3D ( 'NONE', #10017, #10252, #8200 ) ;
#16618 = LINE ( 'NONE', #2673, #21779 ) ;
#16619 = CARTESIAN_POINT ( 'NONE',  ( -44.80746418436748968, 137.9031948627972781, 90.00000000000000000 ) ) ;
#16620 = CARTESIAN_POINT ( 'NONE',  ( 281.4928932188134354, 267.8000000000000114, -150.1999999999999318 ) ) ;
#16621 = ORIENTED_EDGE ( 'NONE', *, *, #4552, .F. ) ;
#16622 = CARTESIAN_POINT ( 'NONE',  ( -8.055391459054613179, -976.2768473852549960, 145.0000119999999697 ) ) ;
#16623 = EDGE_LOOP ( 'NONE', ( #1705, #6489, #8265, #10273 ) ) ;
#16624 = CARTESIAN_POINT ( 'NONE',  ( -6.259644161404860030E-16, -4.618802153517027165, -3.433295621305388234 ) ) ;
#16625 = CARTESIAN_POINT ( 'NONE',  ( 146.4449999999997658, -209.9999999999996874, 30.00000000000641975 ) ) ;
#16626 = ORIENTED_EDGE ( 'NONE', *, *, #12166, .T. ) ;
#16627 = CARTESIAN_POINT ( 'NONE',  ( -282.2000000000012960, -74.99999999999899103, -90.00000000000000000 ) ) ;
#16628 = CARTESIAN_POINT ( 'NONE',  ( 123.2631315123078366, -1093.974511992577163, -28.46977261728505937 ) ) ;
#16629 = DIRECTION ( 'NONE',  ( 0.000000000000000000, 0.000000000000000000, -1.000000000000000000 ) ) ;
#16630 = LINE ( 'NONE', #13035, #11362 ) ;
#16631 = CARTESIAN_POINT ( 'NONE',  ( -7.500000000000005329, 4.330127018922187432, -7.564335161054492218 ) ) ;
#16632 = CARTESIAN_POINT ( 'NONE',  ( -4.000000000000000000, -0.7890432684750890990, -0.04868663549882315533 ) ) ;
#16633 = CARTESIAN_POINT ( 'NONE',  ( 11.07878015919986758, 22.47082401081930669, 145.0000119999999697 ) ) ;
#16634 = ORIENTED_EDGE ( 'NONE', *, *, #18145, .T. ) ;
#16635 = VERTEX_POINT ( 'NONE', #17437 ) ;
#16636 = CARTESIAN_POINT ( 'NONE',  ( 2.000000000000005329, -3.464101615137751722, 0.000000000000000000 ) ) ;
#16637 = DIRECTION ( 'NONE',  ( 0.000000000000000000, 0.000000000000000000, 1.000000000000000000 ) ) ;
#16638 = ORIENTED_EDGE ( 'NONE', *, *, #11288, .F. ) ;
#16639 = ADVANCED_FACE ( 'NONE', ( #879 ), #14661, .T. ) ;
#16640 = ADVANCED_FACE ( 'NONE', ( #1706 ), #23451, .F. ) ;
#16641 = LINE ( 'NONE', #3812, #7734 ) ;
#16642 = CYLINDRICAL_SURFACE ( 'NONE', #19179, 7.500000000000007105 ) ;
#16643 = CARTESIAN_POINT ( 'NONE',  ( 281.9771302778490281, 268.7755403010747841, -146.0571734979477014 ) ) ;
#16644 = ORIENTED_EDGE ( 'NONE', *, *, #8640, .F. ) ;
#16645 = DIRECTION ( 'NONE',  ( 0.000000000000000000, 0.000000000000000000, 1.000000000000000000 ) ) ;
#16646 = CARTESIAN_POINT ( 'NONE',  ( -4.000000000000000000, 0.3987449864459974846, -0.01220643443059782861 ) ) ;
#16647 =( REPRESENTATION_RELATIONSHIP ('NONE','NONE', #10127, #18083 ) REPRESENTATION_RELATIONSHIP_WITH_TRANSFORMATION ( #7538 )SHAPE_REPRESENTATION_RELATIONSHIP( ) );
#16648 = PLANE ( 'NONE',  #23093 ) ;
#16649 = ORIENTED_EDGE ( 'NONE', *, *, #3943, .T. ) ;
#16650 = CARTESIAN_POINT ( 'NONE',  ( 281.4928932188133217, -129.2000000000000455, 177.2000000000014097 ) ) ;
#16651 = LINE ( 'NONE', #16410, #1148 ) ;
#16652 = LINE ( 'NONE', #7576, #21755 ) ;
#16653 = VERTEX_POINT ( 'NONE', #16235 ) ;
#16654 = ORIENTED_EDGE ( 'NONE', *, *, #21682, .T. ) ;
#16655 = SHAPE_DEFINITION_REPRESENTATION ( #9235, #6236 ) ;
#16656 = CARTESIAN_POINT ( 'NONE',  ( -127.2684398464540863, 88.47467185906484133, -27.75009929603929493 ) ) ;
#16657 = DIRECTION ( 'NONE',  ( -1.000000000000000000, -0.000000000000000000, -0.000000000000000000 ) ) ;
#16658 = CARTESIAN_POINT ( 'NONE',  ( -32.35000000000002984, 90.00000000000001421, 3.000000000000001332 ) ) ;
#16659 = ORIENTED_EDGE ( 'NONE', *, *, #2337, .F. ) ;
#16660 = CARTESIAN_POINT ( 'NONE',  ( -24.20041621714726077, -6.482064212728086972, 145.0000119999999697 ) ) ;
#16661 = EDGE_CURVE ( 'NONE', #18758, #5006, #19946, .T. ) ;
#16662 = EDGE_CURVE ( 'NONE', #15218, #15087, #16340, .T. ) ;
#16663 = EDGE_CURVE ( 'NONE', #14713, #8328, #17214, .T. ) ;
#16664 = UNCERTAINTY_MEASURE_WITH_UNIT (LENGTH_MEASURE( 1.000000000000000082E-05 ), #20960, 'distance_accuracy_value', 'NONE');
#16665 = CARTESIAN_POINT ( 'NONE',  ( 0.000000000000000000, 0.000000000000000000, 90.00000000000000000 ) ) ;
#16666 = PLANE ( 'NONE',  #10307 ) ;
#16667 = ORIENTED_EDGE ( 'NONE', *, *, #6658, .T. ) ;
#16668 = LINE ( 'NONE', #9315, #2535 ) ;
#16669 = EDGE_CURVE ( 'NONE', #9425, #12339, #22001, .T. ) ;
#16670 = EDGE_CURVE ( 'NONE', #6504, #18582, #23371, .T. ) ;
#16671 = AXIS2_PLACEMENT_3D ( 'NONE', #21625, #6647, #14041 ) ;
#16672 = ORIENTED_EDGE ( 'NONE', *, *, #9476, .T. ) ;
#16673 = FACE_OUTER_BOUND ( 'NONE', #17163, .T. ) ;
#16674 = CARTESIAN_POINT ( 'NONE',  ( -90.00000000000000000, -74.99999999999998579, 3.000000000000000000 ) ) ;
#16675 = ORIENTED_EDGE ( 'NONE', *, *, #7698, .F. ) ;
#16676 = DIRECTION ( 'NONE',  ( 0.000000000000000000, 0.000000000000000000, 1.000000000000000000 ) ) ;
#16677 = EDGE_CURVE ( 'NONE', #10702, #1956, #17234, .T. ) ;
#16678 = DIRECTION ( 'NONE',  ( -0.000000000000000000, 3.469446951953613794E-15, 1.000000000000000000 ) ) ;
#16679 = CARTESIAN_POINT ( 'NONE',  ( -8.055391459054604297, -1023.723152614744549, 145.0000119999999981 ) ) ;
#16680 = CARTESIAN_POINT ( 'NONE',  ( -280.5724317483737309, 269.9290760626066117, -145.2497115627124060 ) ) ;
#16681 = CARTESIAN_POINT ( 'NONE',  ( 125.7677891478055301, -1090.595098045220993, -31.25700618919319851 ) ) ;
#16682 = DIRECTION ( 'NONE',  ( 0.000000000000000000, -0.000000000000000000, 1.000000000000000000 ) ) ;
#16683 = ORIENTED_EDGE ( 'NONE', *, *, #14191, .T. ) ;
#16684 = DIRECTION ( 'NONE',  ( 0.000000000000000000, 0.5000000000000011102, 0.8660254037844380415 ) ) ;
#16685 = DIRECTION ( 'NONE',  ( 1.000000000000000000, 0.000000000000000000, 0.000000000000000000 ) ) ;
#16686 = FILL_AREA_STYLE ('',( #5687 ) ) ;
#16687 = CIRCLE ( 'NONE', #5889, 2.649999999999985700 ) ;
#16689 = ORIENTED_EDGE ( 'NONE', *, *, #4728, .F. ) ;
#16688 = ORIENTED_EDGE ( 'NONE', *, *, #15337, .T. ) ;
#16690 = CARTESIAN_POINT ( 'NONE',  ( -44.99999999999999289, 240.0000000000000000, 0.000000000000000000 ) ) ;
#16691 = CARTESIAN_POINT ( 'NONE',  ( 5.200000000000002842, 3.306546357697854226E-16, 2.700000000000000622 ) ) ;
#16692 = CARTESIAN_POINT ( 'NONE',  ( 281.4928932188134354, 267.8000000000000114, -147.1999999999999318 ) ) ;
#16693 = ORIENTED_EDGE ( 'NONE', *, *, #9571, .T. ) ;
#16694 = CARTESIAN_POINT ( 'NONE',  ( -100.0000000000000853, -127.0000000000000568, 152.4000000000014268 ) ) ;
#16695 = ORIENTED_EDGE ( 'NONE', *, *, #15278, .F. ) ;
#16696 = EDGE_CURVE ( 'NONE', #18832, #10884, #10929, .T. ) ;
#16697 = CARTESIAN_POINT ( 'NONE',  ( 284.5132312761075468, 270.4054396500289954, -145.9953931959807676 ) ) ;
#16698 = ADVANCED_FACE ( 'NONE', ( #20176 ), #3627, .F. ) ;
#16699 = ORIENTED_EDGE ( 'NONE', *, *, #11998, .T. ) ;
#16700 = ADVANCED_FACE ( 'NONE', ( #12518 ), #21764, .T. ) ;
#16701 = CARTESIAN_POINT ( 'NONE',  ( 40.00000000000000000, 100.0000000000000000, 150.2000000000009550 ) ) ;
#16702 = CARTESIAN_POINT ( 'NONE',  ( 25.00000000000004974, -52.79999999999973426, 35.00000000000017764 ) ) ;
#16703 = ORIENTED_EDGE ( 'NONE', *, *, #8122, .T. ) ;
#16704 = VECTOR ( 'NONE', #6461, 1000.000000000000000 ) ;
#16705 = EDGE_CURVE ( 'NONE', #22268, #19341, #21463, .T. ) ;
#16706 = ADVANCED_FACE ( 'NONE', ( #5226 ), #7263, .F. ) ;
#16707 = CARTESIAN_POINT ( 'NONE',  ( 125.9551925347493722, -1090.334326554368772, 30.33200430454450114 ) ) ;
#16708 = ORIENTED_EDGE ( 'NONE', *, *, #20075, .F. ) ;
#16709 = EDGE_CURVE ( 'NONE', #6984, #21880, #23764, .T. ) ;
#16710 = CARTESIAN_POINT ( 'NONE',  ( 24.99995073929424194, -998.3579766121645207, -145.0000000000001137 ) ) ;
#16711 = CARTESIAN_POINT ( 'NONE',  ( 0.000000000000000000, 0.000000000000000000, -100.0000000000000000 ) ) ;
#16712 = CARTESIAN_POINT ( 'NONE',  ( 2.500000000000002220, 2.357898499370434386, -3.469446951953614189E-15 ) ) ;
#16713 = DIRECTION ( 'NONE',  ( 1.000000000000000000, -0.000000000000000000, -0.000000000000000000 ) ) ;
#16714 = CARTESIAN_POINT ( 'NONE',  ( -79.99999999999995737, -62.00000000000004263, 3.000000000000000000 ) ) ;
#16715 = SURFACE_SIDE_STYLE ('',( #9115 ) ) ;
#16716 = ORIENTED_EDGE ( 'NONE', *, *, #19678, .F. ) ;
#16717 = CIRCLE ( 'NONE', #22870, 5.249999999999949374 ) ;
#16718 = DIRECTION ( 'NONE',  ( 0.000000000000000000, -0.5000000000000009992, -0.8660254037844380415 ) ) ;
#16719 = CARTESIAN_POINT ( 'NONE',  ( 131.8501689178089293, 81.48954978393982174, -28.33934113061009086 ) ) ;
#16720 = CIRCLE ( 'NONE', #6302, 10.12668159690567649 ) ;
#16721 = ORIENTED_EDGE ( 'NONE', *, *, #16734, .T. ) ;
#16722 = LINE ( 'NONE', #10718, #15424 ) ;
#16723 = CARTESIAN_POINT ( 'NONE',  ( -282.6339272673398000, 272.3699028110927429, -145.4976310729377929 ) ) ;
#16724 = CARTESIAN_POINT ( 'NONE',  ( 0.000000000000000000, 5.051668046482832750E-16, -4.000000000000000000 ) ) ;
#16725 = DIRECTION ( 'NONE',  ( 0.000000000000000000, -0.5000000000000013323, -0.8660254037844380415 ) ) ;
#16726 = CARTESIAN_POINT ( 'NONE',  ( -10.00000000000000000, 1.224646799147353256E-15, -50.00000000000000000 ) ) ;
#16727 = VERTEX_POINT ( 'NONE', #18026 ) ;
#16728 = CARTESIAN_POINT ( 'NONE',  ( -23.72315261474501824, -991.9446085409454099, 145.0000119999999697 ) ) ;
#16729 = ORIENTED_EDGE ( 'NONE', *, *, #4999, .T. ) ;
#16730 = LINE ( 'NONE', #661, #5247 ) ;
#16731 = VECTOR ( 'NONE', #6035, 1000.000000000000000 ) ;
#16732 = DIRECTION ( 'NONE',  ( -1.000000000000000000, -0.000000000000000000, -0.000000000000000000 ) ) ;
#16733 = EDGE_CURVE ( 'NONE', #4339, #15682, #19520, .T. ) ;
#16734 = EDGE_CURVE ( 'NONE', #15162, #9146, #12412, .T. ) ;
#16735 = DIRECTION ( 'NONE',  ( -1.000000000000000000, -0.000000000000000000, -0.000000000000000000 ) ) ;
#16736 = ORIENTED_EDGE ( 'NONE', *, *, #5943, .F. ) ;
#16737 = DIRECTION ( 'NONE',  ( 0.000000000000000000, 0.000000000000000000, -1.000000000000000000 ) ) ;
#16738 = CARTESIAN_POINT ( 'NONE',  ( -282.2000000000012960, -74.99999999999899103, -90.00000000000000000 ) ) ;
#16739 = DIRECTION ( 'NONE',  ( -1.110223024625155594E-14, 0.000000000000000000, -1.000000000000000000 ) ) ;
#16740 = DIRECTION ( 'NONE',  ( 0.000000000000000000, -1.000000000000000000, 0.000000000000000000 ) ) ;
#16741 = DIRECTION ( 'NONE',  ( 0.000000000000000000, 0.000000000000000000, 1.000000000000000000 ) ) ;
#16742 = CARTESIAN_POINT ( 'NONE',  ( -7.500000000000698996, 1.613867362005801054, -7.450195926347907616 ) ) ;
#16743 = VERTEX_POINT ( 'NONE', #8739 ) ;
#16744 = CARTESIAN_POINT ( 'NONE',  ( 0.000000000000000000, 5.068713431065766803E-13, 147.2000000000009550 ) ) ;
#16745 = DIRECTION ( 'NONE',  ( -1.350636282998972974E-14, 0.000000000000000000, -1.000000000000000000 ) ) ;
#16746 = ORIENTED_EDGE ( 'NONE', *, *, #15634, .F. ) ;
#16747 = FACE_OUTER_BOUND ( 'NONE', #15860, .T. ) ;
#16749 = AXIS2_PLACEMENT_3D ( 'NONE', #8995, #17928, #16354 ) ;
#16748 = CARTESIAN_POINT ( 'NONE',  ( 5.088535779737119569, -5.722386535631984295, -7.491772860715834703 ) ) ;
#16750 = VECTOR ( 'NONE', #11134, 1000.000000000000000 ) ;
#16751 = CARTESIAN_POINT ( 'NONE',  ( 235.0000000000000284, -500.0000000000000000, 57.00000000000001421 ) ) ;
#16752 = ORIENTED_EDGE ( 'NONE', *, *, #6902, .T. ) ;
#16753 = FACE_OUTER_BOUND ( 'NONE', #11394, .T. ) ;
#16754 = CYLINDRICAL_SURFACE ( 'NONE', #10921, 9.999999999999998224 ) ;
#16755 = CARTESIAN_POINT ( 'NONE',  ( -5.007715329123872641E-16, -8.660254037844399733, -10.00000000000000000 ) ) ;
#16756 = ORIENTED_EDGE ( 'NONE', *, *, #22785, .T. ) ;
#16757 = CARTESIAN_POINT ( 'NONE',  ( 280.0627246244600883, 272.9999999999999432, 145.3431883566701117 ) ) ;
#16758 = DIRECTION ( 'NONE',  ( -0.000000000000000000, -0.000000000000000000, 1.000000000000000000 ) ) ;
#16759 = CIRCLE ( 'NONE', #22694, 2.649999999999971934 ) ;
#16760 = FILL_AREA_STYLE_COLOUR ( '', #7474 ) ;
#16761 = ORIENTED_EDGE ( 'NONE', *, *, #14743, .F. ) ;
#16762 = CARTESIAN_POINT ( 'NONE',  ( 281.3610889986682082, 272.8646579186752774, -145.2488155364688680 ) ) ;
#16763 = APPLICATION_PROTOCOL_DEFINITION ( 'draft international standard', 'automotive_design', 1998, #3955 ) ;
#16764 = CYLINDRICAL_SURFACE ( 'NONE', #19290, 5.199999999999982414 ) ;
#16765 = AXIS2_PLACEMENT_3D ( 'NONE', #6582, #20159, #8626 ) ;
#16766 = DIRECTION ( 'NONE',  ( 0.000000000000000000, -1.000000000000000000, -4.694093751100962712E-16 ) ) ;
#16767 = FACE_OUTER_BOUND ( 'NONE', #10070, .T. ) ;
#16768 = VECTOR ( 'NONE', #13957, 1000.000000000000000 ) ;
#16769 = VECTOR ( 'NONE', #1272, 1000.000000000000000 ) ;
#16770 = ORIENTED_EDGE ( 'NONE', *, *, #8150, .T. ) ;
#16771 = ORIENTED_EDGE ( 'NONE', *, *, #18856, .T. ) ;
#16772 = DIRECTION ( 'NONE',  ( -0.7071067811865416886, 9.961996129952529179E-15, -0.7071067811865532349 ) ) ;
#16773 = PRODUCT_DEFINITION_CONTEXT ( 'detailed design', #12972, 'design' ) ;
#16774 =( REPRESENTATION_RELATIONSHIP ('NONE','NONE', #10127, #22995 ) REPRESENTATION_RELATIONSHIP_WITH_TRANSFORMATION ( #10298 )SHAPE_REPRESENTATION_RELATIONSHIP( ) );
#16775 = APPLICATION_CONTEXT ( 'automotive_design' ) ;
#16776 = DIRECTION ( 'NONE',  ( 0.000000000000000000, 0.000000000000000000, -1.000000000000000000 ) ) ;
#16777 = TOROIDAL_SURFACE ( 'NONE', #4040, 4.000000000000000000, 0.2500000000000000000 ) ;
#16778 = DIRECTION ( 'NONE',  ( 0.000000000000000000, 0.000000000000000000, 1.000000000000000000 ) ) ;
#16779 = VERTEX_POINT ( 'NONE', #16104 ) ;
#16780 = DIRECTION ( 'NONE',  ( 0.000000000000000000, -1.000000000000000000, 0.000000000000000000 ) ) ;
#16781 = EDGE_CURVE ( 'NONE', #11584, #9973, #21654, .T. ) ;
#16782 = AXIS2_PLACEMENT_3D ( 'NONE', #8944, #3789, #5975 ) ;
#16783 = VERTEX_POINT ( 'NONE', #3750 ) ;
#16784 = CARTESIAN_POINT ( 'NONE',  ( 2.500000000000000000, 1.178949249685213863, -2.042000000000001148 ) ) ;
#16785 = ORIENTED_EDGE ( 'NONE', *, *, #991, .F. ) ;
#16786 = CARTESIAN_POINT ( 'NONE',  ( -7.499999999999999112, 41.99999999999998579, 100.0000000000000000 ) ) ;
#16787 = ADVANCED_FACE ( 'NONE', ( #4247 ), #13799, .F. ) ;
#16788 = CARTESIAN_POINT ( 'NONE',  ( -146.0000000000000853, -204.4690652294807478, 30.00000000000641620 ) ) ;
#16789 = CARTESIAN_POINT ( 'NONE',  ( -3.272451888078288906, -1024.838847803014232, 145.0000119999999981 ) ) ;
#16790 = EDGE_CURVE ( 'NONE', #4025, #15178, #14166, .T. ) ;
#16791 = CARTESIAN_POINT ( 'NONE',  ( 155.0000000000000284, -500.0000000000000000, 32.64999999999999858 ) ) ;
#16792 = CARTESIAN_POINT ( 'NONE',  ( 125.8877979345642615, -1090.428239381491721, -29.18615827854500822 ) ) ;
#16793 = LINE ( 'NONE', #15002, #1100 ) ;
#16794 = ORIENTED_EDGE ( 'NONE', *, *, #4305, .T. ) ;
#16795 = DIRECTION ( 'NONE',  ( 0.000000000000000000, 0.8660254037844380415, -0.5000000000000011102 ) ) ;
#16796 = FACE_BOUND ( 'NONE', #21536, .T. ) ;
#16797 = EDGE_CURVE ( 'NONE', #12326, #6747, #5655, .T. ) ;
#16798 = AXIS2_PLACEMENT_3D ( 'NONE', #1488, #16246, #23347 ) ;
#16800 = VERTEX_POINT ( 'NONE', #3987 ) ;
#16799 = ORIENTED_EDGE ( 'NONE', *, *, #19447, .F. ) ;
#16801 = CIRCLE ( 'NONE', #6390, 2.649999999999999467 ) ;
#16802 = B_SPLINE_CURVE_WITH_KNOTS ( 'NONE', 3,
 ( #20844, #11822, #2592, #22986, #4529, #10220, #13871, #11703 ),
 .UNSPECIFIED., .F., .F.,
 ( 4, 2, 2, 4 ),
 ( 0.000000000000000000, 0.002450665683189818828, 0.003675998524784728459, 0.004901331366379638524 ),
 .UNSPECIFIED. ) ;
#16803 = CARTESIAN_POINT ( 'NONE',  ( -135.9487776228375253, -1074.451030117129676, -27.51610016701187078 ) ) ;
#16804 = DIRECTION ( 'NONE',  ( 0.000000000000000000, 0.000000000000000000, -1.000000000000000000 ) ) ;
#16805 = VERTEX_POINT ( 'NONE', #9701 ) ;
#16806 = LINE ( 'NONE', #5577, #9913 ) ;
#16807 = VERTEX_POINT ( 'NONE', #2058 ) ;
#16808 = CIRCLE ( 'NONE', #14503, 2.649999999999985700 ) ;
#16809 = DIRECTION ( 'NONE',  ( -1.000000000000000000, 1.408839003528726857E-14, 6.982962677686266711E-15 ) ) ;
#16810 = ORIENTED_EDGE ( 'NONE', *, *, #18027, .T. ) ;
#16811 = CIRCLE ( 'NONE', #17568, 7.500000000000000000 ) ;
#16812 = CARTESIAN_POINT ( 'NONE',  ( -135.4018704341557964, 51.87806360044768894, -90.00000000000000000 ) ) ;
#16813 = CARTESIAN_POINT ( 'NONE',  ( -7.922281120364393914, -4.573931137438277617, -8.047472243342932430 ) ) ;
#16814 = ORIENTED_EDGE ( 'NONE', *, *, #7716, .T. ) ;
#16815 = AXIS2_PLACEMENT_3D ( 'NONE', #13242, #3997, #11902 ) ;
#16816 = CARTESIAN_POINT ( 'NONE',  ( 125.9265396616754629, -1090.374350352354213, 29.34395718620176297 ) ) ;
#16817 = ORIENTED_EDGE ( 'NONE', *, *, #13498, .F. ) ;
#16818 = CARTESIAN_POINT ( 'NONE',  ( -280.3120962995436685, 272.7324007871374079, 146.6810649015077388 ) ) ;
#16819 = SURFACE_STYLE_FILL_AREA ( #15027 ) ;
#16820 = DIRECTION ( 'NONE',  ( -1.000000000000000000, 1.408839003528726857E-14, 6.982962677686266711E-15 ) ) ;
#16821 = EDGE_CURVE ( 'NONE', #20854, #4839, #9527, .T. ) ;
#16822 = CARTESIAN_POINT ( 'NONE',  ( 0.000000000000000000, 0.000000000000000000, 0.000000000000000000 ) ) ;
#16823 = ORIENTED_EDGE ( 'NONE', *, *, #8783, .F. ) ;
#16824 = CARTESIAN_POINT ( 'NONE',  ( -24.99999999999998224, -1000.000000000000000, 138.9999999999999716 ) ) ;
#16825 = VECTOR ( 'NONE', #16964, 1000.000000000000000 ) ;
#16826 = FILL_AREA_STYLE ('',( #18272 ) ) ;
#16827 = EDGE_CURVE ( 'NONE', #22490, #21286, #10291, .T. ) ;
#16828 = EDGE_CURVE ( 'NONE', #2027, #3977, #20290, .T. ) ;
#16829 = ORIENTED_EDGE ( 'NONE', *, *, #12859, .T. ) ;
#16830 = FILL_AREA_STYLE_COLOUR ( '', #6934 ) ;
#16831 = CIRCLE ( 'NONE', #4091, 20.00000000000000000 ) ;
#16832 = LINE ( 'NONE', #11428, #20049 ) ;
#16833 = CARTESIAN_POINT ( 'NONE',  ( 132.7558223547129046, 80.00574117445245292, -27.49999999999351630 ) ) ;
#16834 = EDGE_CURVE ( 'NONE', #10471, #10559, #16806, .T. ) ;
#16835 = DIRECTION ( 'NONE',  ( -1.000000000000000000, 0.000000000000000000, 0.000000000000000000 ) ) ;
#16836 = CARTESIAN_POINT ( 'NONE',  ( -282.2000000000000455, 269.9999999999999432, -146.4928932188134070 ) ) ;
#16837 = PRODUCT_DEFINITION ( 'UNKNOWN', '', #20063, #2024 ) ;
#16838 = CIRCLE ( 'NONE', #18001, 155.0000000000000284 ) ;
#16839 = DIRECTION ( 'NONE',  ( 1.000000000000000000, 0.000000000000000000, 0.000000000000000000 ) ) ;
#16840 = CARTESIAN_POINT ( 'NONE',  ( 146.0000000000002558, -210.0000000000003411, -32.05499999999356930 ) ) ;
#16841 = EDGE_LOOP ( 'NONE', ( #1106, #22035, #11346, #14583 ) ) ;
#16842 = CARTESIAN_POINT ( 'NONE',  ( -65.00000000000000000, -52.79999999999933635, 155.0000000000001421 ) ) ;
#16843 = ORIENTED_EDGE ( 'NONE', *, *, #23653, .T. ) ;
#16844 = CARTESIAN_POINT ( 'NONE',  ( 34.99999999999999289, 90.00000000000000000, 0.000000000000000000 ) ) ;
#16845 = PLANE ( 'NONE',  #7516 ) ;
#16846 = CARTESIAN_POINT ( 'NONE',  ( 110.0000000000000000, -74.99999999999998579, 3.000000000000000000 ) ) ;
#16847 = VERTEX_POINT ( 'NONE', #15255 ) ;
#16848 = DIRECTION ( 'NONE',  ( -0.000000000000000000, -1.000000000000000000, -0.000000000000000000 ) ) ;
#16849 = CARTESIAN_POINT ( 'NONE',  ( -2.688821387764050996E-14, -4.618802153517012954, -0.4999999999999995559 ) ) ;
#16850 = DIRECTION ( 'NONE',  ( 0.000000000000000000, 0.000000000000000000, -1.000000000000000000 ) ) ;
#16851 = CARTESIAN_POINT ( 'NONE',  ( 1.680279846884594175E-14, -52.79999999999984794, 1.831306136874101946E-13 ) ) ;
#16852 = DIRECTION ( 'NONE',  ( -1.000000000000000000, -0.000000000000000000, -0.000000000000000000 ) ) ;
#16853 = CARTESIAN_POINT ( 'NONE',  ( 4.000000000000000000, 2.309401076758497151, -3.433295621305379353 ) ) ;
#16854 = VECTOR ( 'NONE', #16772, 1000.000000000000114 ) ;
#16855 = CARTESIAN_POINT ( 'NONE',  ( -2.999999999999995559, 0.000000000000000000, 0.000000000000000000 ) ) ;
#16856 = ORIENTED_EDGE ( 'NONE', *, *, #1199, .F. ) ;
#16857 = FACE_BOUND ( 'NONE', #20820, .T. ) ;
#16858 = CIRCLE ( 'NONE', #13814, 5.249999999999973355 ) ;
#16859 = CARTESIAN_POINT ( 'NONE',  ( -64.99999999999995737, -56.79999999999964899, 65.00000000000018474 ) ) ;
#16860 = ORIENTED_EDGE ( 'NONE', *, *, #6665, .T. ) ;
#16861 = ORIENTED_EDGE ( 'NONE', *, *, #12038, .F. ) ;
#16862 = CARTESIAN_POINT ( 'NONE',  ( 2.500000000000002220, 2.357898499370434386, -3.469446951953614189E-15 ) ) ;
#16863 = DIRECTION ( 'NONE',  ( 0.000000000000000000, 0.000000000000000000, 1.000000000000000000 ) ) ;
#16864 = EDGE_CURVE ( 'NONE', #12773, #15576, #13449, .T. ) ;
#16865 = ADVANCED_FACE ( 'NONE', ( #13344 ), #12646, .F. ) ;
#16866 = CARTESIAN_POINT ( 'NONE',  ( 155.0000000000000284, -210.0000000000003411, -29.99999999999350564 ) ) ;
#16867 = ORIENTED_EDGE ( 'NONE', *, *, #16663, .F. ) ;
#16868 = CARTESIAN_POINT ( 'NONE',  ( 5.000000000000004441, 5.204748896376250699E-16, -4.250000000000000000 ) ) ;
#16869 = LINE ( 'NONE', #23754, #486 ) ;
#16870 = CIRCLE ( 'NONE', #1036, 24.69999999999999929 ) ;
#16871 = DIRECTION ( 'NONE',  ( 0.000000000000000000, -4.183096374613631247E-18, -1.000000000000000000 ) ) ;
#16872 = ORIENTED_EDGE ( 'NONE', *, *, #14604, .T. ) ;
#16873 = LINE ( 'NONE', #7820, #12203 ) ;
#16874 = FACE_OUTER_BOUND ( 'NONE', #21649, .T. ) ;
#16875 = CIRCLE ( 'NONE', #19176, 2.055000000000000160 ) ;
#16876 = DIRECTION ( 'NONE',  ( 1.000000000000000000, 0.000000000000000000, 0.000000000000000000 ) ) ;
#16877 = AXIS2_PLACEMENT_3D ( 'NONE', #22095, #5566, #23441 ) ;
#16878 = VERTEX_POINT ( 'NONE', #18836 ) ;
#16879 = CYLINDRICAL_SURFACE ( 'NONE', #11166, 2.500000000000002220 ) ;
#16880 = CIRCLE ( 'NONE', #8402, 2.055000000000001492 ) ;
#16881 = APPLICATION_PROTOCOL_DEFINITION ( 'draft international standard', 'automotive_design', 1998, #16017 ) ;
#16882 = CARTESIAN_POINT ( 'NONE',  ( -1.500000000000000000, 0.000000000000000000, 200.2421591959677016 ) ) ;
#16883 = CARTESIAN_POINT ( 'NONE',  ( -285.2000000000013529, -89.99999999999897682, 21.68333333333335844 ) ) ;
#16884 = CARTESIAN_POINT ( 'NONE',  ( 72.64999999999999147, -87.33333333333332860, 148.0000000000000000 ) ) ;
#16885 = B_SPLINE_CURVE_WITH_KNOTS ( 'NONE', 3,
 ( #23766, #7222, #9410, #11011, #21731, #18445 ),
 .UNSPECIFIED., .F., .F.,
 ( 4, 2, 4 ),
 ( 0.003358874760055551890, 0.004541967308452098118, 0.005725059856848645212 ),
 .UNSPECIFIED. ) ;
#16886 = EDGE_LOOP ( 'NONE', ( #17595, #22504, #1778, #9851 ) ) ;
#16887 = ORIENTED_EDGE ( 'NONE', *, *, #8157, .T. ) ;
#16888 = DIRECTION ( 'NONE',  ( 1.000000000000000000, 0.000000000000000000, 0.000000000000000000 ) ) ;
#16889 = DIRECTION ( 'NONE',  ( 0.000000000000000000, 0.000000000000000000, 1.000000000000000000 ) ) ;
#16890 = VECTOR ( 'NONE', #17358, 1000.000000000000000 ) ;
#16891 = ADVANCED_FACE ( 'NONE', ( #2312, #511 ), #7869, .T. ) ;
#16892 = AXIS2_PLACEMENT_3D ( 'NONE', #6731, #7976, #10507 ) ;
#16893 = CIRCLE ( 'NONE', #23053, 7.500000000000000000 ) ;
#16894 = CIRCLE ( 'NONE', #11132, 1.500000000000001332 ) ;
#16895 = ORIENTED_EDGE ( 'NONE', *, *, #8010, .F. ) ;
#16896 = LINE ( 'NONE', #22320, #13761 ) ;
#16897 = CIRCLE ( 'NONE', #22680, 2.649999999999985700 ) ;
#16898 = EDGE_CURVE ( 'NONE', #16800, #4175, #13704, .T. ) ;
#16899 = CARTESIAN_POINT ( 'NONE',  ( -127.4422799395779009, 88.22408193900459139, 27.62610291900639581 ) ) ;
#16900 = EDGE_LOOP ( 'NONE', ( #8455, #4119, #22819, #17583 ) ) ;
#16901 = CARTESIAN_POINT ( 'NONE',  ( 5.000000000000000000, -4.685197434473811207, 4.770489558936219510E-15 ) ) ;
#16902 = ORIENTED_EDGE ( 'NONE', *, *, #21837, .F. ) ;
#16903 = FILL_AREA_STYLE ('',( #7847 ) ) ;
#16904 = DIRECTION ( 'NONE',  ( 0.000000000000000000, 1.000000000000000000, 0.000000000000000000 ) ) ;
#16905 = VERTEX_POINT ( 'NONE', #8231 ) ;
#16906 = VERTEX_POINT ( 'NONE', #8343 ) ;
#16907 = CARTESIAN_POINT ( 'NONE',  ( -129.1311602790084123, 85.73302760282720669, -31.25700618919315232 ) ) ;
#16908 = AXIS2_PLACEMENT_3D ( 'NONE', #23013, #6483, #11976 ) ;
#16909 = FACE_OUTER_BOUND ( 'NONE', #8228, .T. ) ;
#16910 = VECTOR ( 'NONE', #15430, 1000.000000000000000 ) ;
#16911 = CARTESIAN_POINT ( 'NONE',  ( -24.84002319585407292, -1003.266795291467361, -145.0000000000001137 ) ) ;
#16912 = AXIS2_PLACEMENT_3D ( 'NONE', #2440, #5948, #13358 ) ;
#16913 = CARTESIAN_POINT ( 'NONE',  ( -77.72886158240795851, -117.3074641843678876, -90.00000000000000000 ) ) ;
#16914 = DIRECTION ( 'NONE',  ( 1.000000000000000000, 0.000000000000000000, 0.000000000000000000 ) ) ;
#16915 = LINE ( 'NONE', #15240, #3548 ) ;
#16916 = AXIS2_PLACEMENT_3D ( 'NONE', #16221, #10304, #3268 ) ;
#16917 = CARTESIAN_POINT ( 'NONE',  ( 2.345747346278113987, -3.264484291692503870, -0.01223254789874484924 ) ) ;
#16918 = ORIENTED_EDGE ( 'NONE', *, *, #2680, .F. ) ;
#16919 = CARTESIAN_POINT ( 'NONE',  ( 0.000000000000000000, 0.000000000000000000, -90.00000000000000000 ) ) ;
#16920 = DIRECTION ( 'NONE',  ( 1.000000000000000000, -0.000000000000000000, 6.982962677686266711E-15 ) ) ;
#16921 = VECTOR ( 'NONE', #13296, 1000.000000000000000 ) ;
#16922 = ADVANCED_FACE ( 'NONE', ( #8471 ), #14049, .F. ) ;
#16924 = ORIENTED_EDGE ( 'NONE', *, *, #19053, .F. ) ;
#16923 = ORIENTED_EDGE ( 'NONE', *, *, #3404, .T. ) ;
#16925 = ADVANCED_FACE ( 'NONE', ( #6653 ), #17773, .F. ) ;
#16926 = LINE ( 'NONE', #22353, #13563 ) ;
#16927 = CARTESIAN_POINT ( 'NONE',  ( 280.9952621458755857, 270.4188186979286570, -149.5436892194421148 ) ) ;
#16928 = ORIENTED_EDGE ( 'NONE', *, *, #12294, .T. ) ;
#16929 = EDGE_CURVE ( 'NONE', #6553, #13453, #4605, .T. ) ;
#16930 = VECTOR ( 'NONE', #19004, 1000.000000000000000 ) ;
#16931 = CARTESIAN_POINT ( 'NONE',  ( -135.1744136729186039, -1075.847854466910576, 27.82811892742367021 ) ) ;
#16933 = VECTOR ( 'NONE', #15626, 1000.000000000000000 ) ;
#16932 =( GEOMETRIC_REPRESENTATION_CONTEXT ( 3 ) GLOBAL_UNCERTAINTY_ASSIGNED_CONTEXT ( ( #18789 ) ) GLOBAL_UNIT_ASSIGNED_CONTEXT ( ( #15956, #8467, #23297 ) ) REPRESENTATION_CONTEXT ( 'NONE', 'WORKASPACE' ) );
#16934 = ORIENTED_EDGE ( 'NONE', *, *, #14030, .F. ) ;
#16935 = AXIS2_PLACEMENT_3D ( 'NONE', #8557, #8925, #21342 ) ;
#16936 = CARTESIAN_POINT ( 'NONE',  ( 50.00000000000000000, -62.00000000000001421, 5.199999999999997513 ) ) ;
#16937 = VECTOR ( 'NONE', #51, 1000.000000000000000 ) ;
#16938 = VECTOR ( 'NONE', #5880, 999.9999999999998863 ) ;
#16939 = ORIENTED_EDGE ( 'NONE', *, *, #1073, .F. ) ;
#16940 = LINE ( 'NONE', #13474, #10419 ) ;
#16941 = EDGE_CURVE ( 'NONE', #13423, #8654, #18364, .T. ) ;
#16942 = AXIS2_PLACEMENT_3D ( 'NONE', #10723, #17945, #12089 ) ;
#16943 = ORIENTED_EDGE ( 'NONE', *, *, #21410, .T. ) ;
#16944 = CARTESIAN_POINT ( 'NONE',  ( 3.000000000000002220, 0.000000000000000000, -20.30000000000000071 ) ) ;
#16945 = VERTEX_POINT ( 'NONE', #1217 ) ;
#16946 = CARTESIAN_POINT ( 'NONE',  ( 24.84002319571782280, -996.7332047080466282, -145.0000000000001137 ) ) ;
#16947 = CARTESIAN_POINT ( 'NONE',  ( -7.499999999999999112, 41.99999999999998579, -100.0000000000000000 ) ) ;
#16948 = AXIS2_PLACEMENT_3D ( 'NONE', #9351, #7884, #2325 ) ;
#16949 = DIRECTION ( 'NONE',  ( 0.000000000000000000, 1.000000000000000000, 0.000000000000000000 ) ) ;
#16950 = ORIENTED_EDGE ( 'NONE', *, *, #2513, .F. ) ;
#16952 = CIRCLE ( 'NONE', #21597, 2.649999999999985700 ) ;
#16951 =( GEOMETRIC_REPRESENTATION_CONTEXT ( 3 ) GLOBAL_UNCERTAINTY_ASSIGNED_CONTEXT ( ( #7468 ) ) GLOBAL_UNIT_ASSIGNED_CONTEXT ( ( #10286, #19918, #14504 ) ) REPRESENTATION_CONTEXT ( 'NONE', 'WORKASPACE' ) );
#16953 = CARTESIAN_POINT ( 'NONE',  ( -281.4928932188134354, 267.7999999999999545, -147.1696999999999207 ) ) ;
#16954 = AXIS2_PLACEMENT_3D ( 'NONE', #5128, #16255, #6591 ) ;
#16955 = AXIS2_PLACEMENT_3D ( 'NONE', #74, #189, #14700 ) ;
#16956 = CIRCLE ( 'NONE', #9646, 2.649999999999971934 ) ;
#16957 = CIRCLE ( 'NONE', #13543, 2.055000000000001492 ) ;
#16958 = VERTEX_POINT ( 'NONE', #6185 ) ;
#16959 = DIRECTION ( 'NONE',  ( 1.000000000000000000, 0.000000000000000000, 0.000000000000000000 ) ) ;
#16960 = FACE_OUTER_BOUND ( 'NONE', #15074, .T. ) ;
#16961 = CARTESIAN_POINT ( 'NONE',  ( 132.8404720734533555, 79.86494211668889420, -27.49999999999351985 ) ) ;
#16962 = CARTESIAN_POINT ( 'NONE',  ( 282.1696999999999775, 267.7999999999999545, 146.4928932188134922 ) ) ;
#16963 = EDGE_CURVE ( 'NONE', #12522, #23349, #16447, .T. ) ;
#16964 = DIRECTION ( 'NONE',  ( -0.000000000000000000, -0.000000000000000000, 1.000000000000000000 ) ) ;
#16965 = ADVANCED_FACE ( 'NONE', ( #19552 ), #17293, .F. ) ;
#16966 = ORIENTED_EDGE ( 'NONE', *, *, #21945, .F. ) ;
#16967 = CARTESIAN_POINT ( 'NONE',  ( 30.00000000000000000, 0.000000000000000000, -6.938893903907228378E-15 ) ) ;
#16969 = VECTOR ( 'NONE', #5049, 1000.000000000000114 ) ;
#16968 = AXIS2_PLACEMENT_3D ( 'NONE', #15742, #5222, #7033 ) ;
#16970 = DIRECTION ( 'NONE',  ( 0.000000000000000000, 0.000000000000000000, 1.000000000000000000 ) ) ;
#16971 = CARTESIAN_POINT ( 'NONE',  ( 45.24999999999994316, 100.0000000000000000, -145.0000000000000284 ) ) ;
#16972 = EDGE_CURVE ( 'NONE', #14733, #8946, #6528, .T. ) ;
#16973 = PRESENTATION_LAYER_ASSIGNMENT (  '', '', ( #19268 ) ) ;
#16974 = CIRCLE ( 'NONE', #9663, 0.3000000000000016542 ) ;
#16975 = CONTEXT_DEPENDENT_SHAPE_REPRESENTATION ( #10955, #22959 ) ;
#16976 = VERTEX_POINT ( 'NONE', #18229 ) ;
#16977 = AXIS2_PLACEMENT_3D ( 'NONE', #6284, #9797, #4348 ) ;
#16978 = AXIS2_PLACEMENT_3D ( 'NONE', #18649, #17107, #11456 ) ;
#16979 = CARTESIAN_POINT ( 'NONE',  ( -11.07878015919985160, -977.5291759891805441, 145.0000119999999697 ) ) ;
#16980 = ADVANCED_FACE ( 'NONE', ( #1577 ), #18341, .F. ) ;
#16981 = ORIENTED_EDGE ( 'NONE', *, *, #3928, .F. ) ;
#16982 = DIRECTION ( 'NONE',  ( -1.000000000000000000, 3.495664435217746592E-15, 0.000000000000000000 ) ) ;
#16983 = DIRECTION ( 'NONE',  ( 0.000000000000000000, 0.000000000000000000, -1.000000000000000000 ) ) ;
#16984 = LINE ( 'NONE', #9265, #11006 ) ;
#16985 = VERTEX_POINT ( 'NONE', #1681 ) ;
#16986 = LINE ( 'NONE', #7794, #11958 ) ;
#16987 = AXIS2_PLACEMENT_3D ( 'NONE', #14189, #22966, #10313 ) ;
#16988 = FACE_BOUND ( 'NONE', #18199, .T. ) ;
#16989 = LINE ( 'NONE', #7675, #9614 ) ;
#16990 = EDGE_CURVE ( 'NONE', #13461, #19833, #20152, .T. ) ;
#16991 = CARTESIAN_POINT ( 'NONE',  ( 287.4000000000013415, -132.2000000000000455, -146.4928932188134070 ) ) ;
#16992 = DIRECTION ( 'NONE',  ( -1.000000000000000000, 1.408839003528726857E-14, 6.982962677686266711E-15 ) ) ;
#16993 = CARTESIAN_POINT ( 'NONE',  ( 5.200000000000020606, 3.061616997868392016E-16, -2.500000000000007994 ) ) ;
#16994 = DIRECTION ( 'NONE',  ( 0.000000000000000000, 0.000000000000000000, 1.000000000000000000 ) ) ;
#16995 = ORIENTED_EDGE ( 'NONE', *, *, #19411, .F. ) ;
#16996 = AXIS2_PLACEMENT_3D ( 'NONE', #23289, #4949, #10896 ) ;
#16997 = LINE ( 'NONE', #6113, #4159 ) ;
#16998 = LINE ( 'NONE', #9389, #22734 ) ;
#16999 = EDGE_LOOP ( 'NONE', ( #9702, #18505 ) ) ;
#17000 = AXIS2_PLACEMENT_3D ( 'NONE', #3835, #17127, #20872 ) ;
#17001 = CIRCLE ( 'NONE', #3489, 7.500000000000000888 ) ;
#17002 = VERTEX_POINT ( 'NONE', #5314 ) ;
#17003 = DIRECTION ( 'NONE',  ( 0.000000000000000000, 0.000000000000000000, 1.000000000000000000 ) ) ;
#17004 = LINE ( 'NONE', #2489, #11531 ) ;
#17005 = CARTESIAN_POINT ( 'NONE',  ( 281.9080393212556146, 268.9045205713627524, -145.9942590117596524 ) ) ;
#17006 = ORIENTED_EDGE ( 'NONE', *, *, #20041, .T. ) ;
#17007 = ADVANCED_FACE ( 'NONE', ( #10781 ), #16203, .F. ) ;
#17008 = DIRECTION ( 'NONE',  ( -0.000000000000000000, -1.177509268541832635E-16, 1.000000000000000000 ) ) ;
#17009 = LINE ( 'NONE', #6001, #5872 ) ;
#17010 = EDGE_CURVE ( 'NONE', #3355, #3965, #8957, .T. ) ;
#17011 = CARTESIAN_POINT ( 'NONE',  ( 146.4450000000002490, -801.0618695410406644, -29.99999999999356248 ) ) ;
#17012 = EDGE_CURVE ( 'NONE', #11094, #2904, #16838, .T. ) ;
#17013 = ORIENTED_EDGE ( 'NONE', *, *, #5452, .F. ) ;
#17014 = DIRECTION ( 'NONE',  ( -1.000000000000000000, -0.000000000000000000, -0.000000000000000000 ) ) ;
#17015 = CARTESIAN_POINT ( 'NONE',  ( -288.2000000000010687, -19.99999999999898392, 107.6499999999999631 ) ) ;
#17016 = EDGE_CURVE ( 'NONE', #7318, #15719, #5279, .T. ) ;
#17017 = LINE ( 'NONE', #20603, #8251 ) ;
#17018 = ORIENTED_EDGE ( 'NONE', *, *, #6340, .T. ) ;
#17019 = CARTESIAN_POINT ( 'NONE',  ( 281.3520027839447835, 269.5592670532759030, -145.6220388411722126 ) ) ;
#17020 = PLANE ( 'NONE',  #17000 ) ;
#17021 = EDGE_CURVE ( 'NONE', #22116, #18256, #19688, .T. ) ;
#17022 = EDGE_CURVE ( 'NONE', #18754, #711, #8710, .T. ) ;
#17023 = FACE_OUTER_BOUND ( 'NONE', #11574, .T. ) ;
#17024 = PLANE ( 'NONE',  #15164 ) ;
#17025 = VERTEX_POINT ( 'NONE', #12727 ) ;
#17026 = ORIENTED_EDGE ( 'NONE', *, *, #20857, .T. ) ;
#17027 = FACE_OUTER_BOUND ( 'NONE', #10153, .T. ) ;
#17028 = CARTESIAN_POINT ( 'NONE',  ( -112.7436279071525433, -91.18044947428992941, -90.00000000000000000 ) ) ;
#17029 = CARTESIAN_POINT ( 'NONE',  ( -6.288404560131954923, -5.029641972278938944, -0.4504974108212008721 ) ) ;
#17030 = DIRECTION ( 'NONE',  ( -1.000000000000000000, -0.000000000000000000, -0.000000000000000000 ) ) ;
#17031 = ORIENTED_EDGE ( 'NONE', *, *, #16405, .F. ) ;
#17032 = CARTESIAN_POINT ( 'NONE',  ( -64.99999999999998579, -52.79999999999942872, 125.0000000000001421 ) ) ;
#17033 = ORIENTED_EDGE ( 'NONE', *, *, #21059, .T. ) ;
#17034 = SURFACE_STYLE_FILL_AREA ( #16903 ) ;
#17035 = CARTESIAN_POINT ( 'NONE',  ( -281.4928932188134922, 269.9999999999999432, -147.1999999999999318 ) ) ;
#17036 = ORIENTED_EDGE ( 'NONE', *, *, #6674, .T. ) ;
#17037 = VERTEX_POINT ( 'NONE', #19920 ) ;
#17038 = LINE ( 'NONE', #11753, #7715 ) ;
#17039 = DIRECTION ( 'NONE',  ( 0.000000000000000000, 0.000000000000000000, -1.000000000000000000 ) ) ;
#17040 = ADVANCED_FACE ( 'NONE', ( #1447 ), #14548, .T. ) ;
#17041 = CARTESIAN_POINT ( 'NONE',  ( -90.00000000000000000, -152.9999999999996874, 129.9038105676659711 ) ) ;
#17042 = EDGE_CURVE ( 'NONE', #5315, #6312, #7120, .T. ) ;
#17043 = CARTESIAN_POINT ( 'NONE',  ( -281.6578961534457335, 269.2533442688712171, -145.8089314698393082 ) ) ;
#17044 = CARTESIAN_POINT ( 'NONE',  ( -67.34999999999996589, -87.33333333333338544, 148.0000000000000000 ) ) ;
#17045 = FACE_OUTER_BOUND ( 'NONE', #11893, .T. ) ;
#17046 = CARTESIAN_POINT ( 'NONE',  ( -45.24999999999994316, 100.0000000000000000, 150.2000000000009550 ) ) ;
#17047 = ORIENTED_EDGE ( 'NONE', *, *, #2075, .F. ) ;
#17048 = DIRECTION ( 'NONE',  ( 1.000000000000000000, 0.000000000000000000, 0.000000000000000000 ) ) ;
#17049 = CARTESIAN_POINT ( 'NONE',  ( -7.777900015783941967, -4.169681370001537601, -7.928862157988302073 ) ) ;
#17050 =( NAMED_UNIT ( * ) PLANE_ANGLE_UNIT ( ) SI_UNIT ( $, .RADIAN. ) );
#17051 = ORIENTED_EDGE ( 'NONE', *, *, #10251, .F. ) ;
#17052 = CARTESIAN_POINT ( 'NONE',  ( -136.7463441837909386, -1072.975652424845066, -28.46977261728502384 ) ) ;
#17053 = CARTESIAN_POINT ( 'NONE',  ( 281.2440776823445390, 268.3679143846943589, -147.1132285165672045 ) ) ;
#17054 = ORIENTED_EDGE ( 'NONE', *, *, #5933, .F. ) ;
#17055 = CARTESIAN_POINT ( 'NONE',  ( -134.9759958199650782, -1076.200356551567666, 28.11255663403409244 ) ) ;
#17056 = VERTEX_POINT ( 'NONE', #14511 ) ;
#17057 = B_SPLINE_CURVE_WITH_KNOTS ( 'NONE', 3,
 ( #5813, #5913, #11384, #13324, #18697, #2158, #382, #15124, #20636, #10534, #16067, #19419, #15843, #21486, #23414, #21365, #17763, #5077, #2650, #4950 ),
 .UNSPECIFIED., .F., .F.,
 ( 4, 2, 2, 2, 2, 2, 2, 2, 2, 4 ),
 ( 2.775557561562891043E-17, 0.001035985217005784553, 0.002071970434011541351, 0.003107955651017298149, 0.003625948259520210808, 0.004143940868023123468, 0.005179926085028860316, 0.006215911302034597165, 0.007251896519040333146, 0.008287881736046069994 ),
 .UNSPECIFIED. ) ;
#17058 = DIRECTION ( 'NONE',  ( 0.8090169943749468962, 0.5877852522924740253, 0.000000000000000000 ) ) ;
#17059 = ORIENTED_EDGE ( 'NONE', *, *, #1871, .T. ) ;
#17060 = CARTESIAN_POINT ( 'NONE',  ( -282.2000000000012960, -74.99999999999899103, 90.00000000000000000 ) ) ;
#17061 = CARTESIAN_POINT ( 'NONE',  ( 80.00000000000001421, -56.79999999999913030, 250.0000000000000000 ) ) ;
#17062 = VERTEX_POINT ( 'NONE', #17999 ) ;
#17063 = FACE_OUTER_BOUND ( 'NONE', #13223, .T. ) ;
#17064 = EDGE_LOOP ( 'NONE', ( #6683, #18403, #392, #18978 ) ) ;
#17065 = CARTESIAN_POINT ( 'NONE',  ( 45.00000000000000000, 272.9999999999999432, -5.249999999999973355 ) ) ;
#17066 = DIRECTION ( 'NONE',  ( 0.000000000000000000, 0.000000000000000000, -1.000000000000000000 ) ) ;
#17067 = VECTOR ( 'NONE', #9044, 1000.000000000000000 ) ;
#17068 = DIRECTION ( 'NONE',  ( 0.000000000000000000, -0.000000000000000000, -1.000000000000000000 ) ) ;
#17069 = CARTESIAN_POINT ( 'NONE',  ( -0.2727178028658734932, 0.000000000000000000, 0.000000000000000000 ) ) ;
#17070 = ORIENTED_EDGE ( 'NONE', *, *, #8719, .T. ) ;
#17071 = CARTESIAN_POINT ( 'NONE',  ( -281.9080393212558420, 268.9045205713626956, 145.9942590117597376 ) ) ;
#17072 =( NAMED_UNIT ( * ) SI_UNIT ( $, .STERADIAN. ) SOLID_ANGLE_UNIT ( ) );
#17074 = ORIENTED_EDGE ( 'NONE', *, *, #21580, .F. ) ;
#17073 = VERTEX_POINT ( 'NONE', #15960 ) ;
#17075 = DIRECTION ( 'NONE',  ( 1.000000000000000000, -1.408839003528726857E-14, -6.982962677686266711E-15 ) ) ;
#17076 = DIRECTION ( 'NONE',  ( 1.000000000000000000, 0.000000000000000000, 0.000000000000000000 ) ) ;
#17077 = CARTESIAN_POINT ( 'NONE',  ( 107.6499999999999773, -19.99999999999998934, 3.000000000000001332 ) ) ;
#17078 = DIRECTION ( 'NONE',  ( 0.000000000000000000, 0.000000000000000000, 1.000000000000000000 ) ) ;
#17079 = CARTESIAN_POINT ( 'NONE',  ( -285.2300000000000182, 268.4847249064868606, -146.3684637172358691 ) ) ;
#17080 = EDGE_LOOP ( 'NONE', ( #6161, #23221, #21753, #1772 ) ) ;
#17081 = AXIS2_PLACEMENT_3D ( 'NONE', #7583, #14974, #20736 ) ;
#17082 = LINE ( 'NONE', #2210, #16110 ) ;
#17083 = DIRECTION ( 'NONE',  ( 0.000000000000000000, -1.000000000000000000, 1.287488025362403787E-15 ) ) ;
#17084 = CARTESIAN_POINT ( 'NONE',  ( 122.9460700935429003, -1094.388896850126912, 29.67072815018520515 ) ) ;
#17085 = ORIENTED_EDGE ( 'NONE', *, *, #19631, .F. ) ;
#17086 = DIRECTION ( 'NONE',  ( -1.000000000000000000, -3.469446951953617640E-16, -8.673617379884035472E-17 ) ) ;
#17087 = EDGE_LOOP ( 'NONE', ( #4248, #20204, #20663, #7176 ) ) ;
#17088 = FACE_BOUND ( 'NONE', #3222, .T. ) ;
#17089 = LINE ( 'NONE', #4654, #8324 ) ;
#17090 = ORIENTED_EDGE ( 'NONE', *, *, #999, .F. ) ;
#17091 = DIRECTION ( 'NONE',  ( -1.000000000000000000, -0.000000000000000000, -0.000000000000000000 ) ) ;
#17092 = VERTEX_POINT ( 'NONE', #23303 ) ;
#17093 = CARTESIAN_POINT ( 'NONE',  ( 0.000000000000000000, 0.000000000000000000, -90.00000000000000000 ) ) ;
#17094 = LINE ( 'NONE', #15301, #11922 ) ;
#17095 = EDGE_CURVE ( 'NONE', #6335, #17494, #3599, .T. ) ;
#17096 = CARTESIAN_POINT ( 'NONE',  ( 0.000000000000000000, 0.000000000000000000, -100.0000000000000000 ) ) ;
#17097 = CARTESIAN_POINT ( 'NONE',  ( 3.349226789952652439, 2.685125164760731487, -0.2236248678334773199 ) ) ;
#17098 = DIRECTION ( 'NONE',  ( 6.753181414994864868E-15, 0.000000000000000000, -1.000000000000000000 ) ) ;
#17099 = EDGE_CURVE ( 'NONE', #22918, #21062, #5087, .T. ) ;
#17100 = FACE_OUTER_BOUND ( 'NONE', #20175, .T. ) ;
#17101 = ADVANCED_FACE ( 'NONE', ( #16425 ), #20302, .T. ) ;
#17102 = DIRECTION ( 'NONE',  ( 0.000000000000000000, 0.000000000000000000, 1.000000000000000000 ) ) ;
#17103 = VECTOR ( 'NONE', #3332, 1000.000000000000000 ) ;
#17104 = APPLICATION_CONTEXT ( 'automotive_design' ) ;
#17105 = ORIENTED_EDGE ( 'NONE', *, *, #11341, .T. ) ;
#17106 = FACE_OUTER_BOUND ( 'NONE', #377, .T. ) ;
#17107 = DIRECTION ( 'NONE',  ( 1.000000000000000000, -0.000000000000000000, -0.000000000000000000 ) ) ;
#17108 = EDGE_CURVE ( 'NONE', #21139, #10380, #9125, .T. ) ;
#17109 = VERTEX_POINT ( 'NONE', #23424 ) ;
#17110 = ORIENTED_EDGE ( 'NONE', *, *, #6803, .F. ) ;
#17111 = DIRECTION ( 'NONE',  ( -1.000000000000000000, 0.000000000000000000, 0.000000000000000000 ) ) ;
#17112 = FACE_OUTER_BOUND ( 'NONE', #6308, .T. ) ;
#17113 = LINE ( 'NONE', #7694, #4026 ) ;
#17114 = AXIS2_PLACEMENT_3D ( 'NONE', #15231, #125, #11497 ) ;
#17115 = CIRCLE ( 'NONE', #15582, 2.199999999999979750 ) ;
#17116 = ORIENTED_EDGE ( 'NONE', *, *, #20218, .F. ) ;
#17117 = CYLINDRICAL_SURFACE ( 'NONE', #23454, 5.200000000000031264 ) ;
#17118 = FACE_OUTER_BOUND ( 'NONE', #4103, .T. ) ;
#17119 = CARTESIAN_POINT ( 'NONE',  ( -2.687328764639638656, 3.067272167851286202, -0.05923475698270370959 ) ) ;
#17120 = ORIENTED_EDGE ( 'NONE', *, *, #10223, .T. ) ;
#17121 = DIRECTION ( 'NONE',  ( 1.000000000000000000, 0.000000000000000000, 0.000000000000000000 ) ) ;
#17122 = DIRECTION ( 'NONE',  ( 1.000000000000000000, 0.000000000000000000, 0.000000000000000000 ) ) ;
#17123 = UNCERTAINTY_MEASURE_WITH_UNIT (LENGTH_MEASURE( 1.000000000000000082E-05 ), #8606, 'distance_accuracy_value', 'NONE');
#17124 = SURFACE_STYLE_FILL_AREA ( #18438 ) ;
#17125 = ORIENTED_EDGE ( 'NONE', *, *, #19012, .F. ) ;
#17126 = CARTESIAN_POINT ( 'NONE',  ( 279.9999999999999432, 269.9999999999999432, -144.9999999999999716 ) ) ;
#17127 = DIRECTION ( 'NONE',  ( 0.000000000000000000, 0.000000000000000000, 1.000000000000000000 ) ) ;
#17128 = CARTESIAN_POINT ( 'NONE',  ( 132.8404720734530144, 79.86494211668951948, 32.50000000000646594 ) ) ;
#17129 = CARTESIAN_POINT ( 'NONE',  ( 24.33333333333333215, -89.99999999999998579, 3.000000000000000000 ) ) ;
#17130 = VECTOR ( 'NONE', #3454, 1000.000000000000000 ) ;
#17131 = EDGE_CURVE ( 'NONE', #6254, #13113, #6886, .T. ) ;
#17132 = ORIENTED_EDGE ( 'NONE', *, *, #21274, .T. ) ;
#17133 = AXIS2_PLACEMENT_3D ( 'NONE', #16153, #3207, #8791 ) ;
#17134 = VERTEX_POINT ( 'NONE', #4210 ) ;
#17135 = CARTESIAN_POINT ( 'NONE',  ( 235.0000000000000284, -489.9999999999998863, 60.00000000000000000 ) ) ;
#17136 = PLANE ( 'NONE',  #21405 ) ;
#17137 = ADVANCED_FACE ( 'NONE', ( #2029 ), #3957, .F. ) ;
#17138 = EDGE_CURVE ( 'NONE', #11458, #13550, #18461, .T. ) ;
#17139 = CARTESIAN_POINT ( 'NONE',  ( 4.999999999999997335, 5.204748896376250699E-16, -4.250000000000000000 ) ) ;
#17140 = EDGE_CURVE ( 'NONE', #21238, #22213, #11632, .T. ) ;
#17141 = CARTESIAN_POINT ( 'NONE',  ( -127.0280029979308267, 88.81950979153417336, 28.00660068667234626 ) ) ;
#17142 = EDGE_CURVE ( 'NONE', #10971, #4214, #19534, .T. ) ;
#17143 = ORIENTED_EDGE ( 'NONE', *, *, #10223, .F. ) ;
#17144 = DIRECTION ( 'NONE',  ( 0.000000000000000000, -1.000000000000000000, 0.000000000000000000 ) ) ;
#17145 = VECTOR ( 'NONE', #194, 1000.000000000000000 ) ;
#17146 = ORIENTED_EDGE ( 'NONE', *, *, #19768, .F. ) ;
#17147 = CONICAL_SURFACE ( 'NONE', #22122, 2.041999999999999815, 1.047197551196591858 ) ;
#17148 = DIRECTION ( 'NONE',  ( 0.000000000000000000, 0.000000000000000000, -1.000000000000000000 ) ) ;
#17149 = CARTESIAN_POINT ( 'NONE',  ( -45.00000000000000000, 272.9999999999999432, 0.000000000000000000 ) ) ;
#17150 = ORIENTED_EDGE ( 'NONE', *, *, #22859, .T. ) ;
#17151 = ORIENTED_EDGE ( 'NONE', *, *, #10037, .T. ) ;
#17152 = CARTESIAN_POINT ( 'NONE',  ( -155.0000000000000284, -494.4690652294800088, -27.49999999999350209 ) ) ;
#17153 = VECTOR ( 'NONE', #6414, 1000.000000000000000 ) ;
#17154 = FACE_BOUND ( 'NONE', #14519, .T. ) ;
#17155 = B_SPLINE_CURVE_WITH_KNOTS ( 'NONE', 3,
 ( #23384, #6843, #14245, #21585, #3205, #18406 ),
 .UNSPECIFIED., .F., .F.,
 ( 4, 2, 4 ),
 ( 2.475503369227215526E-07, 0.002222330217055624568, 0.004444412883774326306 ),
 .UNSPECIFIED. ) ;
#17156 = CARTESIAN_POINT ( 'NONE',  ( -6.487492490819623647, -1024.199386683467765, -145.0000000000001137 ) ) ;
#17157 = CARTESIAN_POINT ( 'NONE',  ( 283.9107452280323969, 271.2314821058791949, 145.8083875057489820 ) ) ;
#17158 = CARTESIAN_POINT ( 'NONE',  ( 19.87769063953884441, -984.7502552027949605, 145.0000119999999981 ) ) ;
#17159 = DIRECTION ( 'NONE',  ( -0.000000000000000000, -0.000000000000000000, 1.000000000000000000 ) ) ;
#17160 = ORIENTED_EDGE ( 'NONE', *, *, #13801, .T. ) ;
#17161 = CARTESIAN_POINT ( 'NONE',  ( 0.2791032213812723040, -8.821394357840571132, -7.929128246061910801 ) ) ;
#17162 = AXIS2_PLACEMENT_3D ( 'NONE', #17032, #6026, #10042 ) ;
#17163 = EDGE_LOOP ( 'NONE', ( #9957, #17421, #9808, #19739 ) ) ;
#17164 = CARTESIAN_POINT ( 'NONE',  ( -135.7895026000616951, -1074.740959209979792, -32.49999999999351985 ) ) ;
#17165 = CARTESIAN_POINT ( 'NONE',  ( 80.00000000000000000, -56.79999999999999005, 2.999999999999989786 ) ) ;
#17166 = VECTOR ( 'NONE', #7237, 1000.000000000000000 ) ;
#17167 = VERTEX_POINT ( 'NONE', #10 ) ;
#17168 = CIRCLE ( 'NONE', #6758, 2.649999999999985700 ) ;
#17169 = CARTESIAN_POINT ( 'NONE',  ( -135.4687158836533456, -1075.321440059930865, 27.56549073392519844 ) ) ;
#17170 = EDGE_CURVE ( 'NONE', #11696, #11121, #7988, .T. ) ;
#17171 = EDGE_CURVE ( 'NONE', #11372, #11930, #12266, .T. ) ;
#17172 = VERTEX_POINT ( 'NONE', #14747 ) ;
#17174 = EDGE_CURVE ( 'NONE', #16501, #17172, #20267, .T. ) ;
#17173 = CARTESIAN_POINT ( 'NONE',  ( -40.33333333333332860, -89.99999999999997158, 0.000000000000000000 ) ) ;
#17175 = DIRECTION ( 'NONE',  ( -0.000000000000000000, -0.000000000000000000, 1.000000000000000000 ) ) ;
#17176 = ORIENTED_EDGE ( 'NONE', *, *, #9452, .F. ) ;
#17177 = AXIS2_PLACEMENT_3D ( 'NONE', #17776, #10171, #15614 ) ;
#17178 = CARTESIAN_POINT ( 'NONE',  ( -280.1244294735510607, 272.9999999999999432, 145.6807971656551501 ) ) ;
#17179 = SURFACE_SIDE_STYLE ('',( #22594 ) ) ;
#17180 = ITEM_DEFINED_TRANSFORMATION ( 'NONE', 'NONE', #13171,  #11210 ) ;
#17181 = ORIENTED_EDGE ( 'NONE', *, *, #6246, .F. ) ;
#17182 = FACE_BOUND ( 'NONE', #12424, .T. ) ;
#17183 = EDGE_LOOP ( 'NONE', ( #10394, #411 ) ) ;
#17184 = CARTESIAN_POINT ( 'NONE',  ( 3.266776071109136481, -975.1600734326003703, -145.0000000000001421 ) ) ;
#17185 = CARTESIAN_POINT ( 'NONE',  ( -4.000000000000000000, 2.309401076758498483, -3.433295621305379353 ) ) ;
#17186 = FACE_BOUND ( 'NONE', #22835, .T. ) ;
#17187 = AXIS2_PLACEMENT_3D ( 'NONE', #19919, #8956, #16317 ) ;
#17188 = CARTESIAN_POINT ( 'NONE',  ( 2.500000000000000000, 2.357898499370432166, -2.385244779468109755E-15 ) ) ;
#17189 = ORIENTED_EDGE ( 'NONE', *, *, #14352, .T. ) ;
#17190 = CARTESIAN_POINT ( 'NONE',  ( -280.2488155364688964, 272.8938770989752811, -146.3689414351990479 ) ) ;
#17191 = FILL_AREA_STYLE ('',( #13722 ) ) ;
#17192 = PRODUCT_DEFINITION_SHAPE ( 'NONE', 'NONE',  #23844 ) ;
#17194 = ORIENTED_EDGE ( 'NONE', *, *, #4599, .F. ) ;
#17193 = VERTEX_POINT ( 'NONE', #4080 ) ;
#17195 = CARTESIAN_POINT ( 'NONE',  ( -135.1560209582353025, 94.48200886273060917, 30.00000000000653699 ) ) ;
#17196 = FACE_BOUND ( 'NONE', #8625, .T. ) ;
#17197 = AXIS2_PLACEMENT_3D ( 'NONE', #5265, #9015, #16377 ) ;
#17198 = CARTESIAN_POINT ( 'NONE',  ( 131.5246926503486975, 82.01375679560341325, -29.66799569545553439 ) ) ;
#17199 = CARTESIAN_POINT ( 'NONE',  ( 280.5758453455903805, 269.9427398886703031, 145.2488155364688964 ) ) ;
#17200 = CARTESIAN_POINT ( 'NONE',  ( -31.74999999999995737, 0.000000000000000000, 0.000000000000000000 ) ) ;
#17201 = EDGE_CURVE ( 'NONE', #14920, #436, #18686, .T. ) ;
#17202 = ORIENTED_EDGE ( 'NONE', *, *, #5192, .T. ) ;
#17203 = AXIS2_PLACEMENT_3D ( 'NONE', #21034, #9581, #8243 ) ;
#17204 = PLANE ( 'NONE',  #1442 ) ;
#17205 = EDGE_CURVE ( 'NONE', #12392, #21513, #5903, .T. ) ;
#17206 = CARTESIAN_POINT ( 'NONE',  ( 2.500000000000002220, -1.178949249685215417, 2.042000000000002036 ) ) ;
#17207 = CARTESIAN_POINT ( 'NONE',  ( 123.3278826340506953, -1093.889547229275422, 28.34183984639747322 ) ) ;
#17208 = VERTEX_POINT ( 'NONE', #13080 ) ;
#17209 = DIRECTION ( 'NONE',  ( 0.000000000000000000, -1.000000000000000000, 0.000000000000000000 ) ) ;
#17210 = EDGE_LOOP ( 'NONE', ( #4108, #147, #20634, #10397 ) ) ;
#17211 = DIRECTION ( 'NONE',  ( 0.000000000000000000, 0.000000000000000000, -1.000000000000000000 ) ) ;
#17212 = DIRECTION ( 'NONE',  ( 0.000000000000000000, 0.000000000000000000, -1.000000000000000000 ) ) ;
#17213 = ORIENTED_EDGE ( 'NONE', *, *, #650, .T. ) ;
#17214 = CIRCLE ( 'NONE', #8736, 5.249999999999949374 ) ;
#17215 = CARTESIAN_POINT ( 'NONE',  ( 155.0000000000000284, 2.775557561562891351E-16, -90.00000000000000000 ) ) ;
#17216 = ORIENTED_EDGE ( 'NONE', *, *, #20939, .F. ) ;
#17217 = CARTESIAN_POINT ( 'NONE',  ( -129.6400180686265173, -1072.557589128678728, 27.50000000000641975 ) ) ;
#17218 = CARTESIAN_POINT ( 'NONE',  ( -45.00000000000000000, 272.9999999999999432, 0.000000000000000000 ) ) ;
#17219 = FACE_OUTER_BOUND ( 'NONE', #22471, .T. ) ;
#17220 = CARTESIAN_POINT ( 'NONE',  ( 4.000000000000000000, 2.309401076758497151, -5.000000000000000000 ) ) ;
#17221 = CARTESIAN_POINT ( 'NONE',  ( -285.2000000000007276, 75.00000000000098055, 90.00000000000000000 ) ) ;
#17222 = DIRECTION ( 'NONE',  ( 1.000000000000000000, 0.000000000000000000, 0.000000000000000000 ) ) ;
#17223 = CARTESIAN_POINT ( 'NONE',  ( -7.500000000000000000, -0.7729939684941458111, -7.026407045654831762 ) ) ;
#17224 = ORIENTED_EDGE ( 'NONE', *, *, #17996, .T. ) ;
#17225 =( LENGTH_UNIT ( ) NAMED_UNIT ( * ) SI_UNIT ( .MILLI., .METRE. ) );
#17226 = DIRECTION ( 'NONE',  ( 1.000000000000000000, 0.000000000000000000, 0.000000000000000000 ) ) ;
#17227 = FACE_OUTER_BOUND ( 'NONE', #8506, .T. ) ;
#17228 = ORIENTED_EDGE ( 'NONE', *, *, #8453, .F. ) ;
#17229 = EDGE_CURVE ( 'NONE', #12455, #6451, #6441, .T. ) ;
#17230 = B_SPLINE_CURVE_WITH_KNOTS ( 'NONE', 3,
 ( #8680, #14138, #22823, #13702, #21468, #11766, #19076, #17736 ),
 .UNSPECIFIED., .F., .F.,
 ( 4, 2, 2, 4 ),
 ( 7.780516681398759253E-20, 0.002450665683189819696, 0.003675998524784729327, 0.004901331366379639391 ),
 .UNSPECIFIED. ) ;
#17231 = ORIENTED_EDGE ( 'NONE', *, *, #11895, .T. ) ;
#17232 = DIRECTION ( 'NONE',  ( -1.000000000000000000, -0.000000000000000000, -0.000000000000000000 ) ) ;
#17233 = DIRECTION ( 'NONE',  ( 0.3090169943749441761, 0.9510565162951546414, 0.000000000000000000 ) ) ;
#17234 = CIRCLE ( 'NONE', #642, 5.249999999999949374 ) ;
#17235 = DIRECTION ( 'NONE',  ( 0.000000000000000000, 0.000000000000000000, 1.000000000000000000 ) ) ;
#17236 = EDGE_CURVE ( 'NONE', #1487, #13599, #9313, .T. ) ;
#17237 = ORIENTED_EDGE ( 'NONE', *, *, #23275, .F. ) ;
#17238 = DIRECTION ( 'NONE',  ( -0.000000000000000000, -0.000000000000000000, 1.000000000000000000 ) ) ;
#17239 = CARTESIAN_POINT ( 'NONE',  ( -24.99999999999998224, -52.79999999999934346, 155.0000000000001990 ) ) ;
#17240 = EDGE_CURVE ( 'NONE', #20139, #13908, #11097, .T. ) ;
#17241 = CARTESIAN_POINT ( 'NONE',  ( -25.00000000000000000, 1.865214261513747767E-15, -145.0000119999999697 ) ) ;
#17242 = ORIENTED_EDGE ( 'NONE', *, *, #6169, .F. ) ;
#17243 = CARTESIAN_POINT ( 'NONE',  ( 280.6222583006965010, 271.9268706878667103, 148.1682701916307110 ) ) ;
#17244 = DIRECTION ( 'NONE',  ( 6.640089860198304064E-16, 1.000000000000000000, -3.495664435217746987E-15 ) ) ;
#17245 = ADVANCED_FACE ( 'NONE', ( #20624 ), #16666, .F. ) ;
#17246 = CARTESIAN_POINT ( 'NONE',  ( -155.0000000000000284, -1000.000000000000000, 90.00000000000000000 ) ) ;
#17247 = ORIENTED_EDGE ( 'NONE', *, *, #17171, .T. ) ;
#17248 = AXIS2_PLACEMENT_3D ( 'NONE', #3247, #6650, #6526 ) ;
#17249 = CARTESIAN_POINT ( 'NONE',  ( 80.00000000000004263, -137.9999999999999716, 0.000000000000000000 ) ) ;
#17250 = ITEM_DEFINED_TRANSFORMATION ( 'NONE', 'NONE', #18490,  #11210 ) ;
#17251 = DIRECTION ( 'NONE',  ( -0.000000000000000000, -0.000000000000000000, 1.000000000000000000 ) ) ;
#17252 = AXIS2_PLACEMENT_3D ( 'NONE', #16175, #3476, #14382 ) ;
#17253 = LINE ( 'NONE', #4562, #5744 ) ;
#17254 = PLANE ( 'NONE',  #2794 ) ;
#17255 = UNCERTAINTY_MEASURE_WITH_UNIT (LENGTH_MEASURE( 1.000000000000000082E-05 ), #7946, 'distance_accuracy_value', 'NONE');
#17256 = ORIENTED_EDGE ( 'NONE', *, *, #17960, .T. ) ;
#17257 = ORIENTED_EDGE ( 'NONE', *, *, #9329, .T. ) ;
#17258 = DIRECTION ( 'NONE',  ( -0.000000000000000000, -0.000000000000000000, 1.000000000000000000 ) ) ;
#17259 = DIRECTION ( 'NONE',  ( 0.000000000000000000, 0.000000000000000000, 1.000000000000000000 ) ) ;
#17260 = VECTOR ( 'NONE', #22160, 1000.000000000000000 ) ;
#17261 = ORIENTED_EDGE ( 'NONE', *, *, #4759, .T. ) ;
#17262 = CARTESIAN_POINT ( 'NONE',  ( -110.0000000000000142, 95.00000000000001421, 3.000000000000000000 ) ) ;
#17263 = EDGE_CURVE ( 'NONE', #16229, #6064, #120, .T. ) ;
#17264 = LINE ( 'NONE', #710, #15330 ) ;
#17265 = ORIENTED_EDGE ( 'NONE', *, *, #11557, .T. ) ;
#17266 = EDGE_CURVE ( 'NONE', #67, #5337, #5668, .T. ) ;
#17267 = AXIS2_PLACEMENT_3D ( 'NONE', #7341, #20129, #15528 ) ;
#17268 = CARTESIAN_POINT ( 'NONE',  ( 144.8060344827587187, -7.497491405670202447, 90.00000000000000000 ) ) ;
#17269 = VECTOR ( 'NONE', #12864, 1000.000000000000000 ) ;
#17270 = EDGE_LOOP ( 'NONE', ( #23056, #14008, #1985, #2857, #6883, #9065, #2572 ) ) ;
#17271 = EDGE_CURVE ( 'NONE', #12385, #14070, #5670, .T. ) ;
#17272 = DIRECTION ( 'NONE',  ( 0.000000000000000000, 0.000000000000000000, 1.000000000000000000 ) ) ;
#17273 = ORIENTED_EDGE ( 'NONE', *, *, #18180, .T. ) ;
#17274 = ORIENTED_EDGE ( 'NONE', *, *, #9514, .F. ) ;
#17275 = FACE_BOUND ( 'NONE', #3109, .T. ) ;
#17276 = EDGE_CURVE ( 'NONE', #13152, #4047, #7653, .T. ) ;
#17277 = CARTESIAN_POINT ( 'NONE',  ( 1.828356344711641102, 3.563200125723180900, -5.433716356636336675E-16 ) ) ;
#17278 = AXIS2_PLACEMENT_3D ( 'NONE', #8288, #6347, #16014 ) ;
#17279 = LINE ( 'NONE', #12211, #23051 ) ;
#17280 = CARTESIAN_POINT ( 'NONE',  ( 12.52876685377501964, -978.3042100244117592, 145.0000119999999981 ) ) ;
#17281 = ADVANCED_FACE ( 'NONE', ( #6386 ), #13793, .F. ) ;
#17282 = CARTESIAN_POINT ( 'NONE',  ( 146.4450000000002206, -210.0000000000003411, -29.99999999999356248 ) ) ;
#17283 = VERTEX_POINT ( 'NONE', #2864 ) ;
#17284 = AXIS2_PLACEMENT_3D ( 'NONE', #9703, #5828, #17058 ) ;
#17285 = PLANE ( 'NONE',  #7985 ) ;
#17286 = EDGE_CURVE ( 'NONE', #14316, #3010, #4699, .T. ) ;
#17287 = VECTOR ( 'NONE', #6616, 1000.000000000000114 ) ;
#17288 = AXIS2_PLACEMENT_3D ( 'NONE', #22706, #5064, #13593 ) ;
#17289 = EDGE_LOOP ( 'NONE', ( #6082, #6448, #8163, #22903 ) ) ;
#17290 = FACE_BOUND ( 'NONE', #13170, .T. ) ;
#17291 =( REPRESENTATION_RELATIONSHIP ('NONE','NONE', #10127, #6236 ) REPRESENTATION_RELATIONSHIP_WITH_TRANSFORMATION ( #20083 )SHAPE_REPRESENTATION_RELATIONSHIP( ) );
#17292 = ORIENTED_EDGE ( 'NONE', *, *, #20157, .F. ) ;
#17293 = PLANE ( 'NONE',  #1413 ) ;
#17294 = ORIENTED_EDGE ( 'NONE', *, *, #7058, .F. ) ;
#17295 = CARTESIAN_POINT ( 'NONE',  ( 145.0000000000000284, -500.0000000000000000, -27.49999999999996803 ) ) ;
#17296 = DIRECTION ( 'NONE',  ( 0.9510565162951534202, 0.3090169943749478398, 0.000000000000000000 ) ) ;
#17297 = VERTEX_POINT ( 'NONE', #11996 ) ;
#17298 = EDGE_CURVE ( 'NONE', #12111, #8982, #8211, .T. ) ;
#17299 = AXIS2_PLACEMENT_3D ( 'NONE', #4093, #11506, #23388 ) ;
#17300 = CARTESIAN_POINT ( 'NONE',  ( -280.6220388411723548, 271.9822575857424454, 148.2140793454688037 ) ) ;
#17301 = FILL_AREA_STYLE_COLOUR ( '', #20788 ) ;
#17302 = VECTOR ( 'NONE', #15950, 1000.000000000000000 ) ;
#17303 = ORIENTED_EDGE ( 'NONE', *, *, #10484, .F. ) ;
#17304 = AXIS2_PLACEMENT_3D ( 'NONE', #17824, #1159, #12441 ) ;
#17305 = DIRECTION ( 'NONE',  ( 0.000000000000000000, 0.000000000000000000, 1.000000000000000000 ) ) ;
#17306 = ADVANCED_FACE ( 'NONE', ( #21246 ), #2519, .F. ) ;
#17307 = CARTESIAN_POINT ( 'NONE',  ( -44.99999999999997868, -56.79999999999937188, 192.3500000000001933 ) ) ;
#17308 = CARTESIAN_POINT ( 'NONE',  ( 287.4000000000013415, -127.0000000000000568, 146.4928932188134638 ) ) ;
#17309 = EDGE_CURVE ( 'NONE', #2118, #21406, #17264, .T. ) ;
#17310 = LINE ( 'NONE', #6424, #12352 ) ;
#17311 = EDGE_CURVE ( 'NONE', #7027, #21871, #23779, .T. ) ;
#17312 = ORIENTED_EDGE ( 'NONE', *, *, #17469, .F. ) ;
#17313 = CARTESIAN_POINT ( 'NONE',  ( -281.2440776823445390, 268.3758453455904487, -147.1427398886702349 ) ) ;
#17314 = EDGE_CURVE ( 'NONE', #13252, #3595, #22238, .T. ) ;
#17316 = ORIENTED_EDGE ( 'NONE', *, *, #22197, .T. ) ;
#17315 = ORIENTED_EDGE ( 'NONE', *, *, #3129, .F. ) ;
#17317 = DIRECTION ( 'NONE',  ( 1.000000000000000000, -1.408839003528726857E-14, -6.982962677686266711E-15 ) ) ;
#17318 = VECTOR ( 'NONE', #19256, 1000.000000000000000 ) ;
#17319 = CARTESIAN_POINT ( 'NONE',  ( 7.499999999997997158, -3.157198044624895061, -7.642795354507847527 ) ) ;
#17320 = DIRECTION ( 'NONE',  ( 0.000000000000000000, 0.000000000000000000, 1.000000000000000000 ) ) ;
#17321 = AXIS2_PLACEMENT_3D ( 'NONE', #10203, #4875, #2710 ) ;
#17322 = VECTOR ( 'NONE', #4038, 1000.000000000000000 ) ;
#17323 = CIRCLE ( 'NONE', #21915, 5.200000000000028599 ) ;
#17324 = CARTESIAN_POINT ( 'NONE',  ( 280.5679143846942907, 269.9132285165672442, 145.2488155364688964 ) ) ;
#17325 = DIRECTION ( 'NONE',  ( 0.000000000000000000, -0.5000000000000011102, -0.8660254037844379305 ) ) ;
#17326 = ORIENTED_EDGE ( 'NONE', *, *, #16608, .T. ) ;
#17327 = CONICAL_SURFACE ( 'NONE', #10013, 2.055000000000000160, 0.7853981633974717047 ) ;
#17328 = PLANE ( 'NONE',  #20320 ) ;
#17329 = DIRECTION ( 'NONE',  ( 0.000000000000000000, 1.000000000000000000, 1.224646799147353207E-16 ) ) ;
#17330 = CARTESIAN_POINT ( 'NONE',  ( 279.9999999999999432, 273.0000000000000000, -144.9999999999999716 ) ) ;
#17331 = ORIENTED_EDGE ( 'NONE', *, *, #6643, .F. ) ;
#17332 = DIRECTION ( 'NONE',  ( 0.000000000000000000, -1.000000000000000000, -5.286776307738891306E-15 ) ) ;
#17333 = VERTEX_POINT ( 'NONE', #4458 ) ;
#17335 = CARTESIAN_POINT ( 'NONE',  ( 2.500000000000000000, -2.357898499370432166, 3.035766082959412415E-15 ) ) ;
#17334=STYLED_ITEM('',(#23927),#20059);
#17336 = VECTOR ( 'NONE', #9573, 1000.000000000000000 ) ;
#17337 = FACE_OUTER_BOUND ( 'NONE', #10400, .T. ) ;
#17338 = AXIS2_PLACEMENT_3D ( 'NONE', #980, #10445, #4501 ) ;
#17339 = EDGE_LOOP ( 'NONE', ( #1058, #16716 ) ) ;
#17340 = CIRCLE ( 'NONE', #2283, 145.0000000000000284 ) ;
#17341 = CARTESIAN_POINT ( 'NONE',  ( 11.08413645907697287, 22.46865867799474259, -145.0000000000000000 ) ) ;
#17342 =( GEOMETRIC_REPRESENTATION_CONTEXT ( 3 ) GLOBAL_UNCERTAINTY_ASSIGNED_CONTEXT ( ( #21033 ) ) GLOBAL_UNIT_ASSIGNED_CONTEXT ( ( #2083, #18169, #22380 ) ) REPRESENTATION_CONTEXT ( 'NONE', 'WORKASPACE' ) );
#17343 = ORIENTED_EDGE ( 'NONE', *, *, #11226, .T. ) ;
#17344 = AXIS2_PLACEMENT_3D ( 'NONE', #14691, #9250, #16614 ) ;
#17345 = DIRECTION ( 'NONE',  ( 0.000000000000000000, -0.5000000000000011102, -0.8660254037844379305 ) ) ;
#17346 =( GEOMETRIC_REPRESENTATION_CONTEXT ( 3 ) GLOBAL_UNCERTAINTY_ASSIGNED_CONTEXT ( ( #20875 ) ) GLOBAL_UNIT_ASSIGNED_CONTEXT ( ( #20792, #11528, #9822 ) ) REPRESENTATION_CONTEXT ( 'NONE', 'WORKASPACE' ) );
#17347 = AXIS2_PLACEMENT_3D ( 'NONE', #15676, #4677, #575 ) ;
#17348 = DIRECTION ( 'NONE',  ( 1.000000000000000000, 0.000000000000000000, 0.000000000000000000 ) ) ;
#17349 = CARTESIAN_POINT ( 'NONE',  ( 102.3500000000000085, -19.99999999999998934, 3.000000000000001332 ) ) ;
#17350 = DIRECTION ( 'NONE',  ( 0.000000000000000000, 0.000000000000000000, 1.000000000000000000 ) ) ;
#17351 = EDGE_CURVE ( 'NONE', #5058, #15959, #15589, .T. ) ;
#17352 = LINE ( 'NONE', #21073, #16910 ) ;
#17353 = EDGE_CURVE ( 'NONE', #5058, #19016, #19174, .T. ) ;
#17354 = DIRECTION ( 'NONE',  ( -0.000000000000000000, -1.177509268541832635E-16, 1.000000000000000000 ) ) ;
#17355 = DIRECTION ( 'NONE',  ( 0.000000000000000000, 0.000000000000000000, 1.000000000000000000 ) ) ;
#17356 = EDGE_CURVE ( 'NONE', #8521, #11269, #832, .T. ) ;
#17357 = ORIENTED_EDGE ( 'NONE', *, *, #5050, .F. ) ;
#17358 = DIRECTION ( 'NONE',  ( -0.000000000000000000, -1.000000000000000000, 0.000000000000000000 ) ) ;
#17359 = ORIENTED_EDGE ( 'NONE', *, *, #2551, .F. ) ;
#17360 = ORIENTED_EDGE ( 'NONE', *, *, #4135, .F. ) ;
#17361 = CARTESIAN_POINT ( 'NONE',  ( -1.500000000000000000, 9.886859966642592923, -50.00000000000000000 ) ) ;
#17362 = CARTESIAN_POINT ( 'NONE',  ( -155.0000000000000284, -204.4690652294806057, 27.50000000000647660 ) ) ;
#17364 = AXIS2_PLACEMENT_3D ( 'NONE', #2216, #9856, #16982 ) ;
#17363 = AXIS2_PLACEMENT_3D ( 'NONE', #12894, #11427, #11066 ) ;
#17365 = COLOUR_RGB ( '',1.000000000000000000, 0.9490196078431372140, 0.9098039215686274384 ) ;
#17366 = VECTOR ( 'NONE', #7864, 1000.000000000000000 ) ;
#17367 = CARTESIAN_POINT ( 'NONE',  ( 20.55500000000001748, 3.061616997868384127E-16, -2.500000000000000888 ) ) ;
#17368 = VECTOR ( 'NONE', #10494, 1000.000000000000114 ) ;
#17369 = CARTESIAN_POINT ( 'NONE',  ( 132.6690927018904347, 80.14999981558261766, 27.50000000000646594 ) ) ;
#17370 = CARTESIAN_POINT ( 'NONE',  ( 2.500000000000000000, 2.357898499370431722, -2.818925648462311528E-15 ) ) ;
#17371 = DIRECTION ( 'NONE',  ( -3.051161311199799893E-31, -1.000000000000000000, 0.000000000000000000 ) ) ;
#17372 = ORIENTED_EDGE ( 'NONE', *, *, #17698, .F. ) ;
#17373 = CARTESIAN_POINT ( 'NONE',  ( -79.99999999999995737, -138.0000000000000284, 3.000000000000000000 ) ) ;
#17374 = LINE ( 'NONE', #20602, #8449 ) ;
#17375 = ORIENTED_EDGE ( 'NONE', *, *, #4453, .F. ) ;
#17376 = FACE_OUTER_BOUND ( 'NONE', #2429, .T. ) ;
#17377 = CONTEXT_DEPENDENT_SHAPE_REPRESENTATION ( #2420, #6699 ) ;
#17378 = DIRECTION ( 'NONE',  ( 0.000000000000000000, 0.000000000000000000, 1.000000000000000000 ) ) ;
#17379 = AXIS2_PLACEMENT_3D ( 'NONE', #3621, #14531, #1947 ) ;
#17380 = DIRECTION ( 'NONE',  ( 0.000000000000000000, -3.495664435217746987E-15, 1.000000000000000000 ) ) ;
#17381 = AXIS2_PLACEMENT_3D ( 'NONE', #20349, #16292, #1654 ) ;
#17382 = CARTESIAN_POINT ( 'NONE',  ( -0.5984201754795734907, -8.314755988442763979, -0.7022220667781372549 ) ) ;
#17383 = AXIS2_PLACEMENT_3D ( 'NONE', #10160, #2997, #17867 ) ;
#17384 = VECTOR ( 'NONE', #15903, 1000.000000000000000 ) ;
#17385 = EDGE_CURVE ( 'NONE', #4839, #7372, #10148, .T. ) ;
#17386 = VERTEX_POINT ( 'NONE', #14593 ) ;
#17387 = EDGE_LOOP ( 'NONE', ( #10692, #16995, #22114, #455 ) ) ;
#17388 = DIRECTION ( 'NONE',  ( 0.000000000000000000, 0.000000000000000000, 1.000000000000000000 ) ) ;
#17389 = CARTESIAN_POINT ( 'NONE',  ( 0.000000000000000000, 0.000000000000000000, -90.00000000000000000 ) ) ;
#17390 = ORIENTED_EDGE ( 'NONE', *, *, #219, .F. ) ;
#17391 = ORIENTED_EDGE ( 'NONE', *, *, #22603, .F. ) ;
#17392 = DIRECTION ( 'NONE',  ( -0.3090169943749517811, 0.9510565162951520879, 0.000000000000000000 ) ) ;
#17393 = CARTESIAN_POINT ( 'NONE',  ( -44.80746418436748968, 137.9031948627972781, -90.00000000000000000 ) ) ;
#17394 = CARTESIAN_POINT ( 'NONE',  ( -85.22886158240795851, -117.3074641843678876, 90.00000000000000000 ) ) ;
#17395 = EDGE_LOOP ( 'NONE', ( #19263, #15191, #22557, #5827 ) ) ;
#17396 = CARTESIAN_POINT ( 'NONE',  ( -134.8072682999804499, -1076.498424757946623, -31.52881987646421891 ) ) ;
#17397 = ORIENTED_EDGE ( 'NONE', *, *, #14078, .F. ) ;
#17398 = DIRECTION ( 'NONE',  ( -1.000000000000000000, 7.709882115452476934E-17, 0.000000000000000000 ) ) ;
#17399 = PLANE ( 'NONE',  #16353 ) ;
#17400 = ORIENTED_EDGE ( 'NONE', *, *, #1576, .F. ) ;
#17401 = VERTEX_POINT ( 'NONE', #12584 ) ;
#17402 = CARTESIAN_POINT ( 'NONE',  ( 4.140404888673277384, 2.228338276487440428, -3.686887068327033390 ) ) ;
#17403 = PRODUCT_DEFINITION_SHAPE ( 'NONE', 'NONE',  #23874 ) ;
#17404 = DIRECTION ( 'NONE',  ( 0.000000000000000000, 0.000000000000000000, 1.000000000000000000 ) ) ;
#17405 = CARTESIAN_POINT ( 'NONE',  ( 4.613983237546155358, -6.452243898629820507, -7.591546097228409451 ) ) ;
#17406 = ADVANCED_FACE ( 'NONE', ( #8939 ), #23402, .T. ) ;
#17407 = CARTESIAN_POINT ( 'NONE',  ( -288.2000000000013529, -89.99999999999896261, -37.68333333333335844 ) ) ;
#17408 = ORIENTED_EDGE ( 'NONE', *, *, #22252, .T. ) ;
#17409 = EDGE_CURVE ( 'NONE', #5229, #21974, #16463, .T. ) ;
#17410 = EDGE_LOOP ( 'NONE', ( #14185, #8165, #1066, #15532 ) ) ;
#17411 = EDGE_CURVE ( 'NONE', #16727, #23739, #16858, .T. ) ;
#17412 = VERTEX_POINT ( 'NONE', #10393 ) ;
#17413 = CARTESIAN_POINT ( 'NONE',  ( 15.25452100752526086, -19.87444003240334922, -145.0000000000000000 ) ) ;
#17414 = ORIENTED_EDGE ( 'NONE', *, *, #9075, .F. ) ;
#17415 = CYLINDRICAL_SURFACE ( 'NONE', #21011, 145.0000000000000284 ) ;
#17416 = DIRECTION ( 'NONE',  ( 0.000000000000000000, 0.000000000000000000, 1.000000000000000000 ) ) ;
#17417 = EDGE_LOOP ( 'NONE', ( #2459, #14132 ) ) ;
#17418 = ADVANCED_FACE ( 'NONE', ( #5417 ), #10522, .F. ) ;
#17419 = DIRECTION ( 'NONE',  ( -1.000000000000000000, 3.051161311199799893E-31, 8.144298233840332611E-17 ) ) ;
#17420 = DIRECTION ( 'NONE',  ( -1.110223024625157172E-14, 0.000000000000000000, -1.000000000000000000 ) ) ;
#17421 = ORIENTED_EDGE ( 'NONE', *, *, #16214, .T. ) ;
#17422 = UNCERTAINTY_MEASURE_WITH_UNIT (LENGTH_MEASURE( 1.000000000000000082E-05 ), #16356, 'distance_accuracy_value', 'NONE');
#17423 = FACE_OUTER_BOUND ( 'NONE', #12836, .T. ) ;
#17424 = CARTESIAN_POINT ( 'NONE',  ( 11.08413646075608305, -977.5313413224575925, -145.0000000000001137 ) ) ;
#17425 = CARTESIAN_POINT ( 'NONE',  ( 140.0355749532205607, 37.61698748598765718, 90.00000000000000000 ) ) ;
#17426 = CARTESIAN_POINT ( 'NONE',  ( 285.1999999999999318, 267.7999999999999545, 146.4928932188134922 ) ) ;
#17427 = ORIENTED_EDGE ( 'NONE', *, *, #22741, .F. ) ;
#17428 = DIRECTION ( 'NONE',  ( -1.110223024625157172E-14, 0.000000000000000000, -1.000000000000000000 ) ) ;
#17430 = ORIENTED_EDGE ( 'NONE', *, *, #9440, .T. ) ;
#17429 = VERTEX_POINT ( 'NONE', #17742 ) ;
#17431 = DIRECTION ( 'NONE',  ( -0.6964005597823107463, 0.7176533009294141507, -6.982962677686266711E-15 ) ) ;
#17432 = CARTESIAN_POINT ( 'NONE',  ( 7.894705354777835637, 0.7527931906242791849, -7.590204373988219011 ) ) ;
#17433 = LINE ( 'NONE', #6316, #2326 ) ;
#17434 = EDGE_CURVE ( 'NONE', #19296, #17922, #5621, .T. ) ;
#17435 = EDGE_CURVE ( 'NONE', #17002, #4339, #8568, .T. ) ;
#17436 = LINE ( 'NONE', #17797, #23113 ) ;
#17437 = CARTESIAN_POINT ( 'NONE',  ( -5.007715329123872641E-16, -8.660254037844399733, -7.422398894150038728 ) ) ;
#17438 = ADVANCED_FACE ( 'NONE', ( #1421 ), #3353, .T. ) ;
#17439 = ORIENTED_EDGE ( 'NONE', *, *, #18589, .T. ) ;
#17440 = CARTESIAN_POINT ( 'NONE',  ( -129.6400180686270858, -1072.557589128678273, -27.49999999999356248 ) ) ;
#17441 = EDGE_CURVE ( 'NONE', #23312, #1524, #4936, .T. ) ;
#17442 = PRODUCT_DEFINITION ( 'UNKNOWN', '', #16224, #3953 ) ;
#17443 = CARTESIAN_POINT ( 'NONE',  ( 25.00000000000000000, -1.196402736354634486E-15, -138.9999999999999716 ) ) ;
#17444 = EDGE_CURVE ( 'NONE', #4114, #20274, #6046, .T. ) ;
#17445 = CARTESIAN_POINT ( 'NONE',  ( 123.5484583266988068, -1093.599130927304714, 28.00660068667236757 ) ) ;
#17446 = EDGE_LOOP ( 'NONE', ( #4670, #16506, #11297, #15901 ) ) ;
#17447 = CARTESIAN_POINT ( 'NONE',  ( 153.5653415408403646, -1122.352966361445169, 27.50000000000675371 ) ) ;
#17448 = ORIENTED_EDGE ( 'NONE', *, *, #5631, .T. ) ;
#17449 = DIRECTION ( 'NONE',  ( 2.775557561562891351E-17, -1.000000000000000000, 0.000000000000000000 ) ) ;
#17450 = CARTESIAN_POINT ( 'NONE',  ( -32.35000000000004405, 90.00000000000001421, 0.000000000000000000 ) ) ;
#17451 = ORIENTED_EDGE ( 'NONE', *, *, #21500, .F. ) ;
#17452 = CARTESIAN_POINT ( 'NONE',  ( 24.99995073930944045, 1.642023387880738428, -145.0000000000000284 ) ) ;
#17453 = ORIENTED_EDGE ( 'NONE', *, *, #6248, .T. ) ;
#17454 = FACE_OUTER_BOUND ( 'NONE', #19404, .T. ) ;
#17455 = DIRECTION ( 'NONE',  ( 1.000000000000000000, 0.000000000000000000, 0.000000000000000000 ) ) ;
#17456 = LINE ( 'NONE', #897, #8651 ) ;
#17457 = CARTESIAN_POINT ( 'NONE',  ( 281.9094021484634141, 268.9021437883071712, 145.9954397628184495 ) ) ;
#17458 = LINE ( 'NONE', #11582, #5384 ) ;
#17459 = CARTESIAN_POINT ( 'NONE',  ( -287.4000000000014552, -129.2000000000000455, -146.4928932188134070 ) ) ;
#17460 = ORIENTED_EDGE ( 'NONE', *, *, #1765, .T. ) ;
#17461 = DIRECTION ( 'NONE',  ( -1.000000000000000000, 3.495664435217746987E-15, 0.000000000000000000 ) ) ;
#17462 = CARTESIAN_POINT ( 'NONE',  ( -122.8605704798722940, 82.74225173005859801, 32.05500000000642302 ) ) ;
#17463 = VERTEX_POINT ( 'NONE', #21823 ) ;
#17464 = VECTOR ( 'NONE', #15466, 1000.000000000000000 ) ;
#17465 = ORIENTED_EDGE ( 'NONE', *, *, #17409, .F. ) ;
#17466 = LINE ( 'NONE', #13880, #16169 ) ;
#17467 = DIRECTION ( 'NONE',  ( -0.7232617928448825673, 0.6905739489807055653, 6.982962677686266711E-15 ) ) ;
#17468 = FACE_OUTER_BOUND ( 'NONE', #15225, .T. ) ;
#17469 = EDGE_CURVE ( 'NONE', #8826, #14308, #21479, .T. ) ;
#17470 = EDGE_CURVE ( 'NONE', #15233, #19530, #655, .T. ) ;
#17471 = FACE_OUTER_BOUND ( 'NONE', #16484, .T. ) ;
#17472 = EDGE_CURVE ( 'NONE', #14975, #8155, #5287, .T. ) ;
#17473 = CYLINDRICAL_SURFACE ( 'NONE', #15151, 2.649999999999985700 ) ;
#17474 = DIRECTION ( 'NONE',  ( 0.000000000000000000, 0.000000000000000000, 1.000000000000000000 ) ) ;
#17475 = ORIENTED_EDGE ( 'NONE', *, *, #3655, .T. ) ;
#17476 = LINE ( 'NONE', #920, #12990 ) ;
#17477 = CARTESIAN_POINT ( 'NONE',  ( -146.0000000000001137, -784.4690652294805204, 27.94500000000641649 ) ) ;
#17478 = EDGE_LOOP ( 'NONE', ( #731, #3324, #23252, #13104 ) ) ;
#17479 = CARTESIAN_POINT ( 'NONE',  ( -194.7500000000004832, -784.4690652294792699, -29.99999999999322498 ) ) ;
#17480 = VECTOR ( 'NONE', #5629, 1000.000000000000000 ) ;
#17481 = DIRECTION ( 'NONE',  ( -1.000000000000000000, 0.000000000000000000, 0.000000000000000000 ) ) ;
#17482 = DIRECTION ( 'NONE',  ( 1.000000000000000000, 0.000000000000000000, 0.000000000000000000 ) ) ;
#17483 = DIRECTION ( 'NONE',  ( 1.224646799147353207E-16, 1.000000000000000000, 0.000000000000000000 ) ) ;
#17484 = ORIENTED_EDGE ( 'NONE', *, *, #10775, .T. ) ;
#17485 = EDGE_LOOP ( 'NONE', ( #11543, #6593 ) ) ;
#17486 = FACE_OUTER_BOUND ( 'NONE', #15003, .T. ) ;
#17487 = CARTESIAN_POINT ( 'NONE',  ( -194.7500000000000568, -784.4690652294799520, 27.50000000000675371 ) ) ;
#17488 = ORIENTED_EDGE ( 'NONE', *, *, #22192, .T. ) ;
#17489 = VECTOR ( 'NONE', #17806, 1000.000000000000000 ) ;
#17490 =( GEOMETRIC_REPRESENTATION_CONTEXT ( 3 ) GLOBAL_UNCERTAINTY_ASSIGNED_CONTEXT ( ( #753 ) ) GLOBAL_UNIT_ASSIGNED_CONTEXT ( ( #23433, #6550, #8488 ) ) REPRESENTATION_CONTEXT ( 'NONE', 'WORKASPACE' ) );
#17491 = ORIENTED_EDGE ( 'NONE', *, *, #17236, .T. ) ;
#17492 = DIRECTION ( 'NONE',  ( -1.000000000000000000, 0.000000000000000000, 9.860133695827843917E-17 ) ) ;
#17493 = CARTESIAN_POINT ( 'NONE',  ( -126.6052862049310619, 89.42094583968740551, 28.88679084683406373 ) ) ;
#17494 = VERTEX_POINT ( 'NONE', #23750 ) ;
#17495 = CARTESIAN_POINT ( 'NONE',  ( -135.0351526491288041, -1076.095746396249297, -27.99555145635498477 ) ) ;
#17496 = EDGE_LOOP ( 'NONE', ( #19653, #13997, #18902 ) ) ;
#17497 = CARTESIAN_POINT ( 'NONE',  ( 65.00000000000002842, -52.79999999999929372, 155.0000000000002274 ) ) ;
#17498 = DIRECTION ( 'NONE',  ( 0.000000000000000000, 0.000000000000000000, 1.000000000000000000 ) ) ;
#17499 = ORIENTED_EDGE ( 'NONE', *, *, #12955, .F. ) ;
#17500 = ORIENTED_EDGE ( 'NONE', *, *, #22472, .F. ) ;
#17501 = CARTESIAN_POINT ( 'NONE',  ( 132.8404720734533555, 79.86494211668889420, -27.49999999999351985 ) ) ;
#17502 = AXIS2_PLACEMENT_3D ( 'NONE', #18943, #2404, #491 ) ;
#17503 = DIRECTION ( 'NONE',  ( 0.000000000000000000, 0.000000000000000000, -1.000000000000000000 ) ) ;
#17504 = AXIS2_PLACEMENT_3D ( 'NONE', #5272, #198, #14941 ) ;
#17505 = CARTESIAN_POINT ( 'NONE',  ( -158.1195828810603246, 116.4077317428679947, 30.00000000000675726 ) ) ;
#17506 = VERTEX_POINT ( 'NONE', #17855 ) ;
#17507 = DIRECTION ( 'NONE',  ( 0.000000000000000000, -1.224646799147353454E-16, 1.000000000000000000 ) ) ;
#17508 = EDGE_LOOP ( 'NONE', ( #14783, #15307, #20812, #19687, #9637, #9782, #3528, #17530 ) ) ;
#17509 = ADVANCED_FACE ( 'NONE', ( #1304 ), #16094, .F. ) ;
#17510 = ORIENTED_EDGE ( 'NONE', *, *, #15816, .F. ) ;
#17511 = AXIS2_PLACEMENT_3D ( 'NONE', #4681, #8419, #11846 ) ;
#17512 = CARTESIAN_POINT ( 'NONE',  ( 5.000000000000000000, 4.685197434473814759, -5.637851296924623057E-15 ) ) ;
#17513 = AXIS2_PLACEMENT_3D ( 'NONE', #13989, #23118, #4768 ) ;
#17514 = ORIENTED_EDGE ( 'NONE', *, *, #904, .T. ) ;
#17515 = DIRECTION ( 'NONE',  ( 0.000000000000000000, 0.000000000000000000, -1.000000000000000000 ) ) ;
#17516 = AXIS2_PLACEMENT_3D ( 'NONE', #10751, #18914, #11239 ) ;
#17517 = LINE ( 'NONE', #2676, #595 ) ;
#17518 = EDGE_LOOP ( 'NONE', ( #17375, #12233, #23012, #13783 ) ) ;
#17519 = EDGE_CURVE ( 'NONE', #23739, #21291, #19894, .T. ) ;
#17520 = DIRECTION ( 'NONE',  ( 0.000000000000000000, 0.000000000000000000, -1.000000000000000000 ) ) ;
#17521 = DIRECTION ( 'NONE',  ( -2.238759164535664589E-46, -3.469446951953614189E-15, -1.000000000000000000 ) ) ;
#17522 = EDGE_CURVE ( 'NONE', #16976, #550, #10871, .T. ) ;
#17523 = VERTEX_POINT ( 'NONE', #7783 ) ;
#17524 = CARTESIAN_POINT ( 'NONE',  ( -0.6507732100473471171, 4.243078065514775510, -0.2236248678334823436 ) ) ;
#17525 = LINE ( 'NONE', #18855, #1674 ) ;
#17526 = EDGE_CURVE ( 'NONE', #16062, #2779, #9728, .T. ) ;
#17527 = CYLINDRICAL_SURFACE ( 'NONE', #10365, 145.0000000000000284 ) ;
#17528 = AXIS2_PLACEMENT_3D ( 'NONE', #4285, #22974, #20941 ) ;
#17529 = CARTESIAN_POINT ( 'NONE',  ( 2.500000000000000000, 2.357898499370431722, -2.818925648462311528E-15 ) ) ;
#17530 = ORIENTED_EDGE ( 'NONE', *, *, #11263, .F. ) ;
#17531 = CARTESIAN_POINT ( 'NONE',  ( 0.000000000000000000, 0.000000000000000000, 90.00000000000000000 ) ) ;
#17532 = SURFACE_SIDE_STYLE ('',( #10188 ) ) ;
#17533 = AXIS2_PLACEMENT_3D ( 'NONE', #8351, #19692, #8717 ) ;
#17535 = ORIENTED_EDGE ( 'NONE', *, *, #2203, .F. ) ;
#17534 = EDGE_LOOP ( 'NONE', ( #20865, #16260, #3569, #18809 ) ) ;
#17536 = VECTOR ( 'NONE', #4178, 1000.000000000000000 ) ;
#17537 = DIRECTION ( 'NONE',  ( -6.982962677686266711E-15, 9.837870180509810443E-29, -1.000000000000000000 ) ) ;
#17538 = CARTESIAN_POINT ( 'NONE',  ( -3.750000000000001776, 6.495190528383289141, -6.991905250253753756 ) ) ;
#17539 = CARTESIAN_POINT ( 'NONE',  ( 132.6690927018907473, 80.14999981558196396, -32.49999999999350564 ) ) ;
#17540 = CARTESIAN_POINT ( 'NONE',  ( 0.000000000000000000, 0.000000000000000000, -50.00000000000000000 ) ) ;
#17541 = CARTESIAN_POINT ( 'NONE',  ( -35.00000000000000711, 4.286263797015737285E-15, 100.0000000000000000 ) ) ;
#17542 = DIRECTION ( 'NONE',  ( 1.000000000000000000, 0.000000000000000000, 0.000000000000000000 ) ) ;
#17543 = VERTEX_POINT ( 'NONE', #22747 ) ;
#17544 =( REPRESENTATION_RELATIONSHIP ('NONE','NONE', #10127, #4815 ) REPRESENTATION_RELATIONSHIP_WITH_TRANSFORMATION ( #15328 )SHAPE_REPRESENTATION_RELATIONSHIP( ) );
#17545 = DIRECTION ( 'NONE',  ( -3.051161311199799893E-31, -1.000000000000000000, 0.000000000000000000 ) ) ;
#17546 = CIRCLE ( 'NONE', #15640, 2.055000000000001492 ) ;
#17547 = DIRECTION ( 'NONE',  ( 0.000000000000000000, 0.000000000000000000, 1.000000000000000000 ) ) ;
#17548 =( NAMED_UNIT ( * ) PLANE_ANGLE_UNIT ( ) SI_UNIT ( $, .RADIAN. ) );
#17549 = ITEM_DEFINED_TRANSFORMATION ( 'NONE', 'NONE', #9253,  #11210 ) ;
#17550 = EDGE_LOOP ( 'NONE', ( #17936, #5175, #15208, #854 ) ) ;
#17551 = AXIS2_PLACEMENT_3D ( 'NONE', #5179, #7428, #12481 ) ;
#17552 = CARTESIAN_POINT ( 'NONE',  ( -146.0000000000005116, -204.4690652294800657, -29.99999999999356604 ) ) ;
#17553 = ORIENTED_EDGE ( 'NONE', *, *, #17596, .F. ) ;
#17554 = CARTESIAN_POINT ( 'NONE',  ( -44.99999999999997868, -52.79999999999937899, 142.6500000000001478 ) ) ;
#17555 = DIRECTION ( 'NONE',  ( -1.000000000000000000, -0.000000000000000000, -0.000000000000000000 ) ) ;
#17556 = EDGE_LOOP ( 'NONE', ( #4738, #10157 ) ) ;
#17557 = CARTESIAN_POINT ( 'NONE',  ( 16.51654882469418695, 18.83872056949901008, -145.0000000000000000 ) ) ;
#17558 = EDGE_CURVE ( 'NONE', #4538, #17092, #16875, .T. ) ;
#17559 = CARTESIAN_POINT ( 'NONE',  ( 4.999999999999997335, 0.000000000000000000, 0.000000000000000000 ) ) ;
#17560 = EDGE_CURVE ( 'NONE', #20258, #21638, #2454, .T. ) ;
#17561 = B_SPLINE_CURVE_WITH_KNOTS ( 'NONE', 3,
 ( #11539, #22243, #13134, #18863, #22730, #2330, #11309, #20445, #9716, #17071, #6201, #530, #18615, #6071, #13487, #4269 ),
 .UNSPECIFIED., .F., .F.,
 ( 4, 2, 2, 2, 2, 2, 2, 4 ),
 ( 0.000000000000000000, 0.0009361184303671388424, 0.001404177645550679261, 0.001872236860734219788, 0.002340296075917760316, 0.002808355291101300843, 0.003276414506284841370, 0.003744473721468381464 ),
 .UNSPECIFIED. ) ;
#17562 = DIRECTION ( 'NONE',  ( -1.000000000000000000, -0.000000000000000000, -0.000000000000000000 ) ) ;
#17563 = LINE ( 'NONE', #1011, #1114 ) ;
#17564 = LINE ( 'NONE', #23476, #23501 ) ;
#17565 = DIRECTION ( 'NONE',  ( -1.000000000000000000, 0.000000000000000000, 0.000000000000000000 ) ) ;
#17566 = ADVANCED_FACE ( 'NONE', ( #20935 ), #17204, .F. ) ;
#17567 = ORIENTED_EDGE ( 'NONE', *, *, #12858, .F. ) ;
#17568 = AXIS2_PLACEMENT_3D ( 'NONE', #9911, #20626, #15477 ) ;
#17569 = CARTESIAN_POINT ( 'NONE',  ( -7.640563834021360018E-16, -9.147862274876560562, -8.047472243342937759 ) ) ;
#17570 = CARTESIAN_POINT ( 'NONE',  ( 34.99999999999999289, 2.516649172247811061E-16, -2.055000000000000160 ) ) ;
#17571 = EDGE_CURVE ( 'NONE', #13321, #8675, #14965, .T. ) ;
#17572 = ORIENTED_EDGE ( 'NONE', *, *, #1221, .T. ) ;
#17573 = VECTOR ( 'NONE', #3761, 1000.000000000000000 ) ;
#17574 = ORIENTED_EDGE ( 'NONE', *, *, #7211, .T. ) ;
#17575 = CARTESIAN_POINT ( 'NONE',  ( 117.3074641843663386, 85.22886158241004750, -90.00000000000000000 ) ) ;
#17576 = CARTESIAN_POINT ( 'NONE',  ( 9.999999999999998224, 1.224646799147352862E-15, 200.0000119999999981 ) ) ;
#17578 = CARTESIAN_POINT ( 'NONE',  ( -35.00000000000000000, 0.000000000000000000, -100.0000000000000000 ) ) ;
#17577 = PRODUCT_DEFINITION_SHAPE ( 'NONE', 'NONE',  #23868 ) ;
#17579 = AXIS2_PLACEMENT_3D ( 'NONE', #3435, #5606, #22135 ) ;
#17580 = DIRECTION ( 'NONE',  ( 0.000000000000000000, 0.000000000000000000, 1.000000000000000000 ) ) ;
#17581 = DIRECTION ( 'NONE',  ( -1.350636282998972974E-14, 0.000000000000000000, -1.000000000000000000 ) ) ;
#17582 = CARTESIAN_POINT ( 'NONE',  ( -2.000000000000006661, 3.464101615137750834, 0.000000000000000000 ) ) ;
#17583 = ORIENTED_EDGE ( 'NONE', *, *, #4759, .F. ) ;
#17584 = CARTESIAN_POINT ( 'NONE',  ( 20.00000000000000000, 0.000000000000000000, -150.0000000000000000 ) ) ;
#17585 = FACE_OUTER_BOUND ( 'NONE', #18499, .T. ) ;
#17586 = ADVANCED_FACE ( 'NONE', ( #8156 ), #20822, .F. ) ;
#17587 = DIRECTION ( 'NONE',  ( 0.000000000000000000, 0.8660254037844380415, -0.5000000000000009992 ) ) ;
#17588 = ORIENTED_EDGE ( 'NONE', *, *, #15050, .T. ) ;
#17589 = DIRECTION ( 'NONE',  ( 0.000000000000000000, -1.000000000000000000, 0.000000000000000000 ) ) ;
#17590 = CARTESIAN_POINT ( 'NONE',  ( 99.99999999999987210, -132.2000000000000455, 177.2000000000014097 ) ) ;
#17591 = CARTESIAN_POINT ( 'NONE',  ( -7.500000000000000000, -4.330127018922198090, -7.422398894150034288 ) ) ;
#17592 = CARTESIAN_POINT ( 'NONE',  ( 6.487720807613236218, -1024.199240824787012, -145.0000000000001421 ) ) ;
#17593 = PLANE ( 'NONE',  #2655 ) ;
#17594 = CARTESIAN_POINT ( 'NONE',  ( -285.0327955282141943, 269.1518577254344677, 146.2434055557877741 ) ) ;
#17595 = ORIENTED_EDGE ( 'NONE', *, *, #16669, .F. ) ;
#17597 = EDGE_LOOP ( 'NONE', ( #9162, #19250, #20299, #13441 ) ) ;
#17596 = EDGE_CURVE ( 'NONE', #10369, #21860, #23034, .T. ) ;
#17598 = CARTESIAN_POINT ( 'NONE',  ( 235.0000000000000284, -560.0000000000000000, 59.99999999999999289 ) ) ;
#17599 = AXIS2_PLACEMENT_3D ( 'NONE', #16134, #5138, #11203 ) ;
#17600 = DIRECTION ( 'NONE',  ( 0.000000000000000000, -0.5000000000000012212, -0.8660254037844380415 ) ) ;
#17601 = EDGE_CURVE ( 'NONE', #18021, #20231, #1017, .T. ) ;
#17602 = EDGE_LOOP ( 'NONE', ( #17859, #20552, #7793, #8575 ) ) ;
#17603 = LINE ( 'NONE', #1056, #21235 ) ;
#17604 = AXIS2_PLACEMENT_3D ( 'NONE', #20824, #7784, #14808 ) ;
#17605 = ORIENTED_EDGE ( 'NONE', *, *, #11972, .F. ) ;
#17606 = LINE ( 'NONE', #4457, #9430 ) ;
#17607 = CARTESIAN_POINT ( 'NONE',  ( -126.6511612778954685, 89.35598455390400829, 28.74044610054854942 ) ) ;
#17608 = ORIENTED_EDGE ( 'NONE', *, *, #13798, .F. ) ;
#17609 = CARTESIAN_POINT ( 'NONE',  ( -135.7895026000616951, -1074.740959209979792, -32.49999999999351985 ) ) ;
#17610 = AXIS2_PLACEMENT_3D ( 'NONE', #22579, #11513, #4478 ) ;
#17611 = ORIENTED_EDGE ( 'NONE', *, *, #22876, .F. ) ;
#17612 = VECTOR ( 'NONE', #7016, 1000.000000000000000 ) ;
#17613 = DIRECTION ( 'NONE',  ( 0.000000000000000000, 0.000000000000000000, 1.000000000000000000 ) ) ;
#17614 = DIRECTION ( 'NONE',  ( 0.000000000000000000, 0.000000000000000000, -1.000000000000000000 ) ) ;
#17615 = ORIENTED_EDGE ( 'NONE', *, *, #872, .F. ) ;
#17616 = ORIENTED_EDGE ( 'NONE', *, *, #10885, .T. ) ;
#17617 = CARTESIAN_POINT ( 'NONE',  ( 133.1749347183809675, 79.30613235828936070, -32.42132972170174554 ) ) ;
#17618 = DIRECTION ( 'NONE',  ( -1.000000000000000000, 0.000000000000000000, 0.000000000000000000 ) ) ;
#17619 = FACE_OUTER_BOUND ( 'NONE', #3885, .T. ) ;
#17620 = CARTESIAN_POINT ( 'NONE',  ( -146.4450000000000500, -494.4690652294806910, 32.50000000000641620 ) ) ;
#17621 = AXIS2_PLACEMENT_3D ( 'NONE', #1666, #103, #12253 ) ;
#17622 = VERTEX_POINT ( 'NONE', #13621 ) ;
#17623 = ADVANCED_FACE ( 'NONE', ( #11799 ), #17328, .T. ) ;
#17624 = CARTESIAN_POINT ( 'NONE',  ( -44.99999999999997868, -52.79999999999936477, 195.0000000000001705 ) ) ;
#17625 = CIRCLE ( 'NONE', #22638, 2.041999999999999815 ) ;
#17626 = ORIENTED_EDGE ( 'NONE', *, *, #9723, .F. ) ;
#17627 = EDGE_CURVE ( 'NONE', #20433, #20414, #17640, .T. ) ;
#17628 = AXIS2_PLACEMENT_3D ( 'NONE', #16093, #20283, #16332 ) ;
#17629 = VERTEX_POINT ( 'NONE', #13375 ) ;
#17630 = CARTESIAN_POINT ( 'NONE',  ( 22.46869086673244809, -11.08405874239030275, -145.0000000000000000 ) ) ;
#17631 = ORIENTED_EDGE ( 'NONE', *, *, #9405, .F. ) ;
#17632 = DIRECTION ( 'NONE',  ( 0.000000000000000000, -1.000000000000000000, 0.000000000000000000 ) ) ;
#17633 = CARTESIAN_POINT ( 'NONE',  ( -2.999999999999998668, 2.486033002269127373E-15, 20.30000000000000071 ) ) ;
#17634 = ORIENTED_EDGE ( 'NONE', *, *, #1221, .F. ) ;
#17635 = CARTESIAN_POINT ( 'NONE',  ( -280.6220388411723548, 269.5350371479512432, 146.3333820183295586 ) ) ;
#17636 = CARTESIAN_POINT ( 'NONE',  ( -155.0000000000000284, -204.4690652294806625, 32.50000000000648015 ) ) ;
#17637 = CIRCLE ( 'NONE', #17278, 2.700000000000000622 ) ;
#17638 = ORIENTED_EDGE ( 'NONE', *, *, #19638, .T. ) ;
#17639 = DIRECTION ( 'NONE',  ( -1.000000000000000000, -3.736327486719275871E-16, -0.000000000000000000 ) ) ;
#17640 = CIRCLE ( 'NONE', #7229, 2.649999999999971934 ) ;
#17641 = LINE ( 'NONE', #21506, #1280 ) ;
#17642 = CIRCLE ( 'NONE', #6083, 35.00000000000000000 ) ;
#17643 = FACE_OUTER_BOUND ( 'NONE', #20111, .T. ) ;
#17644 = EDGE_CURVE ( 'NONE', #17092, #4538, #6847, .T. ) ;
#17645 = CIRCLE ( 'NONE', #5313, 2.500000000000000444 ) ;
#17646 = CARTESIAN_POINT ( 'NONE',  ( -129.2206655591611764, -1072.408698320350140, -27.94499999999358053 ) ) ;
#17647 = ADVANCED_BREP_SHAPE_REPRESENTATION ( '', ( #12097, #11210 ), #370 ) ;
#17648 = EDGE_LOOP ( 'NONE', ( #22688, #5341, #10613, #9153 ) ) ;
#17649 = CYLINDRICAL_SURFACE ( 'NONE', #3816, 2.500000000000002220 ) ;
#17650 =( NAMED_UNIT ( * ) PLANE_ANGLE_UNIT ( ) SI_UNIT ( $, .RADIAN. ) );
#17652 = ORIENTED_EDGE ( 'NONE', *, *, #14762, .T. ) ;
#17651 = ORIENTED_EDGE ( 'NONE', *, *, #19929, .F. ) ;
#17653 = EDGE_CURVE ( 'NONE', #5300, #5262, #12682, .T. ) ;
#17654 = DIRECTION ( 'NONE',  ( 0.9873505073845698643, 0.1585527532634884162, -8.221344500052600232E-17 ) ) ;
#17655 = DIRECTION ( 'NONE',  ( -0.9423651898111408132, -0.3345860861306287348, 6.982962677686266711E-15 ) ) ;
#17656 = CARTESIAN_POINT ( 'NONE',  ( 132.4977819882884660, 80.43276747726498854, -32.43450926607475537 ) ) ;
#17657 = VECTOR ( 'NONE', #3306, 1000.000000000000000 ) ;
#17658 = DIRECTION ( 'NONE',  ( 0.000000000000000000, -1.000000000000000000, 0.000000000000000000 ) ) ;
#17659 = LINE ( 'NONE', #990, #13915 ) ;
#17660 = DIRECTION ( 'NONE',  ( 1.110223024625155594E-14, 0.000000000000000000, -1.000000000000000000 ) ) ;
#17661 = AXIS2_PLACEMENT_3D ( 'NONE', #16438, #4977, #23789 ) ;
#17662 = ORIENTED_EDGE ( 'NONE', *, *, #21541, .T. ) ;
#17663 = EDGE_CURVE ( 'NONE', #1796, #12484, #18788, .T. ) ;
#17664 = AXIS2_PLACEMENT_3D ( 'NONE', #20032, #23415, #5081 ) ;
#17665 = DIRECTION ( 'NONE',  ( -1.000000000000000000, -0.000000000000000000, -0.000000000000000000 ) ) ;
#17666 = VECTOR ( 'NONE', #20966, 1000.000000000000000 ) ;
#17667 = ORIENTED_EDGE ( 'NONE', *, *, #7335, .T. ) ;
#17668 = CARTESIAN_POINT ( 'NONE',  ( -281.4928932188134922, -132.2000000000000455, -177.2000000000013529 ) ) ;
#17669 = DIRECTION ( 'NONE',  ( 1.110223024625156383E-14, -1.000000000000000000, 0.000000000000000000 ) ) ;
#17670 = ORIENTED_EDGE ( 'NONE', *, *, #8189, .F. ) ;
#17671 = CARTESIAN_POINT ( 'NONE',  ( -65.00000000000000000, -52.79999999999933635, 155.0000000000001421 ) ) ;
#17672 = VERTEX_POINT ( 'NONE', #10994 ) ;
#17673 = DIRECTION ( 'NONE',  ( -0.000000000000000000, -0.000000000000000000, 1.000000000000000000 ) ) ;
#17674 = CARTESIAN_POINT ( 'NONE',  ( -69.99999999999997158, -112.6666666666667140, 3.000000000000000000 ) ) ;
#17675 = VERTEX_POINT ( 'NONE', #18312 ) ;
#17676 = CARTESIAN_POINT ( 'NONE',  ( -7.894787914004607998, -1.230850257101226302E-13, -7.591390474663425536 ) ) ;
#17677 = PRODUCT_DEFINITION_SHAPE ( 'NONE', 'NONE',  #14645 ) ;
#17678 = AXIS2_PLACEMENT_3D ( 'NONE', #5269, #22151, #9135 ) ;
#17679 = DIRECTION ( 'NONE',  ( 1.000000000000000000, 0.000000000000000000, 0.000000000000000000 ) ) ;
#17680 = DIRECTION ( 'NONE',  ( -0.000000000000000000, -0.000000000000000000, 1.000000000000000000 ) ) ;
#17681 = DIRECTION ( 'NONE',  ( -1.000000000000000000, 0.000000000000000000, 0.000000000000000000 ) ) ;
#17682 = VECTOR ( 'NONE', #6646, 1000.000000000000000 ) ;
#17683 = FACE_OUTER_BOUND ( 'NONE', #14425, .T. ) ;
#17684 = AXIS2_PLACEMENT_3D ( 'NONE', #4856, #21859, #19701 ) ;
#17685 = ORIENTED_EDGE ( 'NONE', *, *, #11731, .F. ) ;
#17686 = EDGE_CURVE ( 'NONE', #5390, #2544, #17082, .T. ) ;
#17687 =( NAMED_UNIT ( * ) SI_UNIT ( $, .STERADIAN. ) SOLID_ANGLE_UNIT ( ) );
#17688 = EDGE_CURVE ( 'NONE', #23173, #20673, #2342, .T. ) ;
#17689 = CARTESIAN_POINT ( 'NONE',  ( -31.74999999999994316, 0.000000000000000000, 0.000000000000000000 ) ) ;
#17690 = PLANE ( 'NONE',  #9665 ) ;
#17691 = CONICAL_SURFACE ( 'NONE', #12014, 7.500000000000001776, 0.8594454914424796144 ) ;
#17692 = VERTEX_POINT ( 'NONE', #8507 ) ;
#17693 = VERTEX_POINT ( 'NONE', #19714 ) ;
#17694 = CARTESIAN_POINT ( 'NONE',  ( -2.500000000000000444, 3.061616997868383634E-16, -5.000000000000000888 ) ) ;
#17695 = CARTESIAN_POINT ( 'NONE',  ( 7.922281120364393914, -4.573931137438282057, -8.047472243342932430 ) ) ;
#17696 = ADVANCED_FACE ( 'NONE', ( #23336 ), #20727, .F. ) ;
#17697 = CARTESIAN_POINT ( 'NONE',  ( 5.000000000000000000, -2.342598717236900718, 4.057500000000001883 ) ) ;
#17698 = EDGE_CURVE ( 'NONE', #20488, #14701, #6572, .T. ) ;
#17699 = CIRCLE ( 'NONE', #6515, 4.250000000000000000 ) ;
#17701 = CIRCLE ( 'NONE', #1882, 2.499999999999998668 ) ;
#17700 = MECHANICAL_DESIGN_GEOMETRIC_PRESENTATION_REPRESENTATION (  '', ( #6534 ), #14280 ) ;
#17702 = AXIS2_PLACEMENT_3D ( 'NONE', #23242, #14107, #1158 ) ;
#17703 = DIRECTION ( 'NONE',  ( -0.5000000000000051070, 0.000000000000000000, 0.8660254037844355990 ) ) ;
#17704 = VECTOR ( 'NONE', #2589, 1000.000000000000000 ) ;
#17705 = CARTESIAN_POINT ( 'NONE',  ( -284.1268706878666990, 270.9682701916306087, -145.8706349181168491 ) ) ;
#17706 = AXIS2_PLACEMENT_3D ( 'NONE', #2623, #8079, #11619 ) ;
#17707 = AXIS2_PLACEMENT_3D ( 'NONE', #1483, #11051, #20183 ) ;
#17708 = VECTOR ( 'NONE', #21990, 1000.000000000000114 ) ;
#17709 = DIRECTION ( 'NONE',  ( 1.000000000000000000, 0.000000000000000000, 0.000000000000000000 ) ) ;
#17710 = ORIENTED_EDGE ( 'NONE', *, *, #16063, .F. ) ;
#17711 = CARTESIAN_POINT ( 'NONE',  ( 171.6502151485116201, 95.33502053007514121, -27.49999999999322498 ) ) ;
#17713 = EDGE_CURVE ( 'NONE', #7849, #6769, #19442, .T. ) ;
#17712 = FACE_OUTER_BOUND ( 'NONE', #16469, .T. ) ;
#17714 = DIRECTION ( 'NONE',  ( 0.000000000000000000, 0.000000000000000000, -1.000000000000000000 ) ) ;
#17715 = VERTEX_POINT ( 'NONE', #23098 ) ;
#17716 = PRESENTATION_STYLE_ASSIGNMENT (( #10370 ) ) ;
#17717 = DIRECTION ( 'NONE',  ( -0.000000000000000000, 1.000000000000000000, -0.000000000000000000 ) ) ;
#17718 = CARTESIAN_POINT ( 'NONE',  ( -280.0000000000000568, 267.7999999999999545, -147.1999999999999318 ) ) ;
#17719 = CARTESIAN_POINT ( 'NONE',  ( 45.00000000000000000, 250.0000000000000000, 0.000000000000000000 ) ) ;
#17720 = LINE ( 'NONE', #21698, #9218 ) ;
#17721 = DIRECTION ( 'NONE',  ( -1.000000000000000000, 0.000000000000000000, -0.000000000000000000 ) ) ;
#17722 = CARTESIAN_POINT ( 'NONE',  ( -1.206569728928481577, -7.963640680051488729, -0.4524126574264552558 ) ) ;
#17723 = EDGE_LOOP ( 'NONE', ( #12200, #63, #18400, #3429 ) ) ;
#17724 = ORIENTED_EDGE ( 'NONE', *, *, #5882, .F. ) ;
#17726 = VECTOR ( 'NONE', #3357, 1000.000000000000000 ) ;
#17725 = AXIS2_PLACEMENT_3D ( 'NONE', #22611, #20814, #6075 ) ;
#17727 = DIRECTION ( 'NONE',  ( 1.000000000000000000, 0.000000000000000000, 0.000000000000000000 ) ) ;
#17728 = LINE ( 'NONE', #23266, #18119 ) ;
#17729 = AXIS2_PLACEMENT_3D ( 'NONE', #3426, #12653, #3302 ) ;
#17730 = CIRCLE ( 'NONE', #1885, 2.649999999999978595 ) ;
#17731 = ORIENTED_EDGE ( 'NONE', *, *, #10824, .F. ) ;
#17732 = CIRCLE ( 'NONE', #6559, 2.499999999999998668 ) ;
#17733 = CIRCLE ( 'NONE', #5387, 7.500000000000001776 ) ;
#17734 = AXIS2_PLACEMENT_3D ( 'NONE', #3447, #19630, #10608 ) ;
#17735 = DIRECTION ( 'NONE',  ( 1.000000000000000000, 0.000000000000000000, 0.000000000000000000 ) ) ;
#17736 = CARTESIAN_POINT ( 'NONE',  ( 4.211140560182196957, 2.431303136016536470, -3.745885042887433514 ) ) ;
#17737 = ADVANCED_FACE ( 'NONE', ( #12161 ), #21407, .T. ) ;
#17738 = EDGE_CURVE ( 'NONE', #20433, #7876, #996, .T. ) ;
#17739 = ORIENTED_EDGE ( 'NONE', *, *, #23482, .T. ) ;
#17740 = CARTESIAN_POINT ( 'NONE',  ( 25.00000000000002132, -52.79999999999930793, 155.0000000000001990 ) ) ;
#17741 = ADVANCED_FACE ( 'NONE', ( #8376 ), #15752, .F. ) ;
#17742 = CARTESIAN_POINT ( 'NONE',  ( 20.00000000000000000, 0.000000000000000000, 124.9999999999999716 ) ) ;
#17743 = ORIENTED_EDGE ( 'NONE', *, *, #1664, .F. ) ;
#17744 = ADVANCED_FACE ( 'NONE', ( #10321, #16106, #13852 ), #21299, .T. ) ;
#17745 = CARTESIAN_POINT ( 'NONE',  ( -134.6768122279369209, -1076.727833257003113, -31.11299551804361130 ) ) ;
#17746 = VERTEX_POINT ( 'NONE', #19350 ) ;
#17747 = EDGE_CURVE ( 'NONE', #12275, #14316, #4750, .T. ) ;
#17749 = AXIS2_PLACEMENT_3D ( 'NONE', #7184, #80, #23619 ) ;
#17748 = AXIS2_PLACEMENT_3D ( 'NONE', #14768, #20288, #21997 ) ;
#17750 = CARTESIAN_POINT ( 'NONE',  ( -37.30746418436748968, 137.9031948627972781, -90.00000000000000000 ) ) ;
#17751 =( REPRESENTATION_RELATIONSHIP ('NONE','NONE', #10127, #4815 ) REPRESENTATION_RELATIONSHIP_WITH_TRANSFORMATION ( #15459 )SHAPE_REPRESENTATION_RELATIONSHIP( ) );
#17752 = EDGE_CURVE ( 'NONE', #550, #10015, #15991, .T. ) ;
#17753 = AXIS2_PLACEMENT_3D ( 'NONE', #9821, #1096, #12031 ) ;
#17754 = PRESENTATION_LAYER_ASSIGNMENT (  '', '', ( #1161 ) ) ;
#17756 = CIRCLE ( 'NONE', #7331, 2.055000000000001492 ) ;
#17755 = CARTESIAN_POINT ( 'NONE',  ( 70.00000000000000000, -112.6666666666666714, 148.0000000000000000 ) ) ;
#17757 = ORIENTED_EDGE ( 'NONE', *, *, #6983, .F. ) ;
#17758 = ORIENTED_EDGE ( 'NONE', *, *, #8752, .F. ) ;
#17759 = CARTESIAN_POINT ( 'NONE',  ( -155.0000000000000284, -204.4690652294800088, -27.49999999999350209 ) ) ;
#17760 = AXIS2_PLACEMENT_3D ( 'NONE', #14303, #4974, #10671 ) ;
#17761 = AXIS2_PLACEMENT_3D ( 'NONE', #1267, #1016, #8398 ) ;
#17762 = DIRECTION ( 'NONE',  ( -0.8823264512277401161, -0.4706379005816069272, 1.080538264299094565E-16 ) ) ;
#17763 = CARTESIAN_POINT ( 'NONE',  ( -281.2434055557877741, 269.1518577254345246, -150.0327955282141659 ) ) ;
#17764 = CARTESIAN_POINT ( 'NONE',  ( -2.352174619740013739, 7.302225387956623237, -7.450218641348505422 ) ) ;
#17765 = CARTESIAN_POINT ( 'NONE',  ( 5.000000000000000888, 0.000000000000000000, -25.03750572909317285 ) ) ;
#17766 = ORIENTED_EDGE ( 'NONE', *, *, #241, .T. ) ;
#17767 = LINE ( 'NONE', #8466, #20684 ) ;
#17768 = VERTEX_POINT ( 'NONE', #2811 ) ;
#17769 = VECTOR ( 'NONE', #15673, 1000.000000000000000 ) ;
#17770 = CIRCLE ( 'NONE', #781, 7.500000000000001776 ) ;
#17771 = VECTOR ( 'NONE', #6433, 1000.000000000000000 ) ;
#17772 = EDGE_LOOP ( 'NONE', ( #16238, #13837, #4404, #14843 ) ) ;
#17773 = PLANE ( 'NONE',  #23394 ) ;
#17774 = ORIENTED_EDGE ( 'NONE', *, *, #11070, .F. ) ;
#17775 = CARTESIAN_POINT ( 'NONE',  ( 5.174575781541291164, 5.672711317429402378, -7.030005583190089169 ) ) ;
#17776 = CARTESIAN_POINT ( 'NONE',  ( 100.0000000000000000, 249.9999999999999716, 125.0000000000000284 ) ) ;
#17777 = ORIENTED_EDGE ( 'NONE', *, *, #23000, .T. ) ;
#17778 = EDGE_CURVE ( 'NONE', #13794, #10166, #4873, .T. ) ;
#17779 = CARTESIAN_POINT ( 'NONE',  ( -136.8702482660834789, -1072.742966597998702, 28.88679084683412768 ) ) ;
#17780 = CARTESIAN_POINT ( 'NONE',  ( 100.0000000000000000, 249.9999999999999716, 145.0000000000000284 ) ) ;
#17781 = ADVANCED_FACE ( 'NONE', ( #14080 ), #19950, .T. ) ;
#17782 = ORIENTED_EDGE ( 'NONE', *, *, #18974, .T. ) ;
#17783 = LINE ( 'NONE', #1225, #15445 ) ;
#17784 = PLANE ( 'NONE',  #9780 ) ;
#17785 = CARTESIAN_POINT ( 'NONE',  ( 121.5574576620405480, -79.04925354955113903, -90.00000000000000000 ) ) ;
#17786 = DIRECTION ( 'NONE',  ( 0.4924295582441687857, -0.5074575156280874966, 0.7071067811865630048 ) ) ;
#17787 = DIRECTION ( 'NONE',  ( 0.000000000000000000, -3.495664435217746987E-15, -1.000000000000000000 ) ) ;
#17788 = VERTEX_POINT ( 'NONE', #17440 ) ;
#17789 = CARTESIAN_POINT ( 'NONE',  ( -31.74999999999995737, 5.204748896376250699E-16, -4.250000000000000000 ) ) ;
#17790 = PRODUCT_DEFINITION_SHAPE ( 'NONE', 'NONE',  #23843 ) ;
#17792 = ORIENTED_EDGE ( 'NONE', *, *, #12035, .T. ) ;
#17791 = ORIENTED_EDGE ( 'NONE', *, *, #16496, .F. ) ;
#17793 = DIRECTION ( 'NONE',  ( 2.832769448823989808E-16, -1.000000000000000000, 3.469446951953613794E-15 ) ) ;
#17794 = CARTESIAN_POINT ( 'NONE',  ( 7.500000000000000000, 1.545478204151513157, -7.491761935628701075 ) ) ;
#17795 = DIRECTION ( 'NONE',  ( -0.000000000000000000, -0.000000000000000000, 1.000000000000000000 ) ) ;
#17796 = CARTESIAN_POINT ( 'NONE',  ( 45.00000000000002132, -52.79999999999936477, 140.0000000000001990 ) ) ;
#17797 = CARTESIAN_POINT ( 'NONE',  ( 37.64999999999996305, 90.00000000000000000, 3.000000000000000000 ) ) ;
#17798 = LINE ( 'NONE', #19458, #8345 ) ;
#17799 = ORIENTED_EDGE ( 'NONE', *, *, #6983, .T. ) ;
#17800 = CARTESIAN_POINT ( 'NONE',  ( 7.499999999999999112, -4.330127018922205195, -1.000000000000000888 ) ) ;
#17801 = ORIENTED_EDGE ( 'NONE', *, *, #3934, .F. ) ;
#17802 = DIRECTION ( 'NONE',  ( -0.000000000000000000, -0.000000000000000000, 1.000000000000000000 ) ) ;
#17803 = LINE ( 'NONE', #14330, #3068 ) ;
#17804 = ITEM_DEFINED_TRANSFORMATION ( 'NONE', 'NONE', #14653,  #11210 ) ;
#17805 = ORIENTED_EDGE ( 'NONE', *, *, #18455, .F. ) ;
#17806 = DIRECTION ( 'NONE',  ( 0.000000000000000000, -1.000000000000000000, 0.000000000000000000 ) ) ;
#17807 = EDGE_LOOP ( 'NONE', ( #6112, #23159, #22564, #13950 ) ) ;
#17808 = CARTESIAN_POINT ( 'NONE',  ( 5.000000000000018652, 0.000000000000000000, -2.700000000000004174 ) ) ;
#17809 = LINE ( 'NONE', #14204, #1367 ) ;
#17810 = ORIENTED_EDGE ( 'NONE', *, *, #9180, .T. ) ;
#17811 = DIRECTION ( 'NONE',  ( 0.000000000000000000, 0.000000000000000000, 1.000000000000000000 ) ) ;
#17812 = DIRECTION ( 'NONE',  ( -0.8660254037844377084, -0.5000000000000015543, 0.000000000000000000 ) ) ;
#17813 = CARTESIAN_POINT ( 'NONE',  ( -7.497491405671719455, 144.8060344827586334, -90.00000000000000000 ) ) ;
#17814 = DIRECTION ( 'NONE',  ( 0.000000000000000000, 0.000000000000000000, 1.000000000000000000 ) ) ;
#17815 = DIRECTION ( 'NONE',  ( 0.000000000000000000, -1.000000000000000000, 0.000000000000000000 ) ) ;
#17816 = DIRECTION ( 'NONE',  ( 1.000000000000000000, 0.000000000000000000, 0.000000000000000000 ) ) ;
#17817 = ORIENTED_EDGE ( 'NONE', *, *, #17012, .T. ) ;
#17818 = SHAPE_REPRESENTATION_RELATIONSHIP ( 'NONE' , 'NONE' ,  #11474, #20508 ) ;
#17819 = DIRECTION ( 'NONE',  ( -1.000000000000000000, -3.469446951953614682E-16, -0.000000000000000000 ) ) ;
#17820 = CARTESIAN_POINT ( 'NONE',  ( -40.00000000000000000, 100.0000000000000000, 145.0000000000000000 ) ) ;
#17821 = ORIENTED_EDGE ( 'NONE', *, *, #9056, .F. ) ;
#17822 = VERTEX_POINT ( 'NONE', #11923 ) ;
#17823 = CARTESIAN_POINT ( 'NONE',  ( 7.499999999999997335, 34.18698582794336005, -100.0000000000000000 ) ) ;
#17824 = CARTESIAN_POINT ( 'NONE',  ( 2.500000000000000000, -1.178949249685213863, 2.042000000000001148 ) ) ;
#17825 = DIRECTION ( 'NONE',  ( 1.000000000000000000, 0.000000000000000000, 0.000000000000000000 ) ) ;
#17826 = DIRECTION ( 'NONE',  ( 0.000000000000000000, 0.000000000000000000, 1.000000000000000000 ) ) ;
#17827 = DIRECTION ( 'NONE',  ( -1.000000000000000000, -0.000000000000000000, -0.000000000000000000 ) ) ;
#17828 = ORIENTED_EDGE ( 'NONE', *, *, #13547, .T. ) ;
#17829 = FACE_BOUND ( 'NONE', #12464, .T. ) ;
#17830 = ORIENTED_EDGE ( 'NONE', *, *, #22167, .T. ) ;
#17831 = EDGE_CURVE ( 'NONE', #13331, #1763, #19236, .T. ) ;
#17832 = CARTESIAN_POINT ( 'NONE',  ( 40.00000000000000000, 100.0000000000000000, -145.0000000000000284 ) ) ;
#17833 = DIRECTION ( 'NONE',  ( 0.000000000000000000, 1.000000000000000000, 0.000000000000000000 ) ) ;
#17834 = EDGE_CURVE ( 'NONE', #4754, #9308, #4535, .T. ) ;
#17835 = EDGE_CURVE ( 'NONE', #8946, #2340, #12414, .T. ) ;
#17836 = ORIENTED_EDGE ( 'NONE', *, *, #3809, .F. ) ;
#17837 = DIRECTION ( 'NONE',  ( 0.000000000000000000, -1.000000000000000000, 0.000000000000000000 ) ) ;
#17838 = DIRECTION ( 'NONE',  ( -1.000000000000000000, -0.000000000000000000, -0.000000000000000000 ) ) ;
#17839 = CARTESIAN_POINT ( 'NONE',  ( -137.9031948627974486, 44.80746418436699940, 90.00000000000000000 ) ) ;
#17840 = DIRECTION ( 'NONE',  ( 1.000000000000000000, 0.000000000000000000, 0.000000000000000000 ) ) ;
#17841 = FACE_OUTER_BOUND ( 'NONE', #13820, .T. ) ;
#17842 = EDGE_CURVE ( 'NONE', #1216, #17073, #1599, .T. ) ;
#17843 = FACE_OUTER_BOUND ( 'NONE', #23198, .T. ) ;
#17844 = CARTESIAN_POINT ( 'NONE',  ( -283.0299054689547802, 272.0295083325148084, 145.5908103165960767 ) ) ;
#17845 = AXIS2_PLACEMENT_3D ( 'NONE', #2742, #11603, #8067 ) ;
#17846 = VERTEX_POINT ( 'NONE', #10930 ) ;
#17847 = ORIENTED_EDGE ( 'NONE', *, *, #22007, .F. ) ;
#17848 = DIRECTION ( 'NONE',  ( 0.000000000000000000, 1.177509268541832635E-16, -1.000000000000000000 ) ) ;
#17849 = CARTESIAN_POINT ( 'NONE',  ( 281.2431816561009441, 268.3724317483736854, 147.1290760626067140 ) ) ;
#17850 = ORIENTED_EDGE ( 'NONE', *, *, #13348, .T. ) ;
#17851 = CARTESIAN_POINT ( 'NONE',  ( 0.000000000000000000, 0.000000000000000000, 0.000000000000000000 ) ) ;
#17852 = FACE_BOUND ( 'NONE', #23755, .T. ) ;
#17853 = ORIENTED_EDGE ( 'NONE', *, *, #16095, .F. ) ;
#17854 = LINE ( 'NONE', #19300, #227 ) ;
#17855 = CARTESIAN_POINT ( 'NONE',  ( -24.99999999999999645, -2.129009867111508370E-15, 145.0000059999999849 ) ) ;
#17856 = EDGE_LOOP ( 'NONE', ( #23206, #332, #13976, #700 ) ) ;
#17857 = DIRECTION ( 'NONE',  ( 0.000000000000000000, 0.000000000000000000, -1.000000000000000000 ) ) ;
#17858 = VECTOR ( 'NONE', #12602, 1000.000000000000000 ) ;
#17859 = ORIENTED_EDGE ( 'NONE', *, *, #18331, .T. ) ;
#17860 = DIRECTION ( 'NONE',  ( 0.000000000000000000, 0.000000000000000000, 1.000000000000000000 ) ) ;
#17861 = LINE ( 'NONE', #21724, #17883 ) ;
#17862 = EDGE_LOOP ( 'NONE', ( #15141, #14477 ) ) ;
#17863 = ORIENTED_EDGE ( 'NONE', *, *, #19170, .F. ) ;
#17864 = CARTESIAN_POINT ( 'NONE',  ( 133.6917068022189596, 78.43176171823509435, -31.88829724122658504 ) ) ;
#17865 = EDGE_CURVE ( 'NONE', #11184, #16172, #19549, .T. ) ;
#17866 = DIRECTION ( 'NONE',  ( 6.123233995736766036E-17, 0.000000000000000000, -1.000000000000000000 ) ) ;
#17867 = DIRECTION ( 'NONE',  ( 1.000000000000000000, 0.000000000000000000, 0.000000000000000000 ) ) ;
#17868 = EDGE_CURVE ( 'NONE', #12504, #13509, #10737, .T. ) ;
#17869 = DIRECTION ( 'NONE',  ( 0.000000000000000000, 0.000000000000000000, 1.000000000000000000 ) ) ;
#17870 = PLANE ( 'NONE',  #16671 ) ;
#17871 = ADVANCED_FACE ( 'NONE', ( #1823 ), #9223, .F. ) ;
#17872 = ORIENTED_EDGE ( 'NONE', *, *, #11142, .T. ) ;
#17873 = DIRECTION ( 'NONE',  ( -1.000000000000000000, -2.775557561562891351E-17, 0.000000000000000000 ) ) ;
#17874 = AXIS2_PLACEMENT_3D ( 'NONE', #16011, #10115, #21076 ) ;
#17875 =( REPRESENTATION_RELATIONSHIP ('NONE','NONE', #10127, #14711 ) REPRESENTATION_RELATIONSHIP_WITH_TRANSFORMATION ( #2923 )SHAPE_REPRESENTATION_RELATIONSHIP( ) );
#17876 = ADVANCED_FACE ( 'NONE', ( #6924 ), #11047, .F. ) ;
#17877 = ORIENTED_EDGE ( 'NONE', *, *, #16574, .T. ) ;
#17878 = EDGE_CURVE ( 'NONE', #19431, #12825, #3629, .T. ) ;
#17879 = EDGE_LOOP ( 'NONE', ( #14018, #1636, #21736, #18210, #2755 ) ) ;
#17880 = CARTESIAN_POINT ( 'NONE',  ( 24.83992656990903569, -3.266860234290754672, -145.0000000000000000 ) ) ;
#17881 = ORIENTED_EDGE ( 'NONE', *, *, #12442, .F. ) ;
#17882 = FACE_OUTER_BOUND ( 'NONE', #10995, .T. ) ;
#17883 = VECTOR ( 'NONE', #20022, 1000.000000000000114 ) ;
#17884 = ORIENTED_EDGE ( 'NONE', *, *, #8783, .T. ) ;
#17885 = PRODUCT ( 'discharge spout', 'discharge spout', '', ( #18794 ) ) ;
#17886 = VECTOR ( 'NONE', #19513, 1000.000000000000000 ) ;
#17887 = CARTESIAN_POINT ( 'NONE',  ( -85.22886158240879695, 117.3074641843673049, -90.00000000000000000 ) ) ;
#17888 = ORIENTED_EDGE ( 'NONE', *, *, #10932, .F. ) ;
#17889 = CARTESIAN_POINT ( 'NONE',  ( 1.734723475976807094E-15, 4.618802153517012954, -0.4999999999999995559 ) ) ;
#17890 = CARTESIAN_POINT ( 'NONE',  ( -7.499999999999999112, 34.18698582794336716, 100.0000000000000000 ) ) ;
#17891 = DIRECTION ( 'NONE',  ( -1.000000000000000000, 0.000000000000000000, 0.000000000000000000 ) ) ;
#17892 = FACE_OUTER_BOUND ( 'NONE', #12264, .T. ) ;
#17893 = CARTESIAN_POINT ( 'NONE',  ( 40.00000000000000000, 100.0000000000000000, 147.2000000000005855 ) ) ;
#17894 = EDGE_LOOP ( 'NONE', ( #15828, #19127, #23466, #20714 ) ) ;
#17895 = CARTESIAN_POINT ( 'NONE',  ( -281.4928932188135491, -132.2000000000000455, 177.2000000000014097 ) ) ;
#17896 = AXIS2_PLACEMENT_3D ( 'NONE', #6257, #19034, #21227 ) ;
#17898 = VERTEX_POINT ( 'NONE', #1955 ) ;
#17897 = ORIENTED_EDGE ( 'NONE', *, *, #3148, .T. ) ;
#17899 = AXIS2_PLACEMENT_3D ( 'NONE', #22242, #20551, #20306 ) ;
#17900 = DIRECTION ( 'NONE',  ( 1.000000000000000000, 0.000000000000000000, 6.123233995736766036E-17 ) ) ;
#17901 = ADVANCED_FACE ( 'NONE', ( #8872 ), #5466, .F. ) ;
#17902 = EDGE_CURVE ( 'NONE', #9425, #14489, #5310, .T. ) ;
#17903 = DIRECTION ( 'NONE',  ( 0.000000000000000000, -1.000000000000000000, 0.000000000000000000 ) ) ;
#17904 = FACE_OUTER_BOUND ( 'NONE', #13141, .T. ) ;
#17905 = ADVANCED_FACE ( 'NONE', ( #5231 ), #9094, .F. ) ;
#17906 = AXIS2_PLACEMENT_3D ( 'NONE', #1680, #14620, #7015 ) ;
#17907 = CARTESIAN_POINT ( 'NONE',  ( 44.80746418436557832, 137.9031948627978750, -90.00000000000000000 ) ) ;
#17908 = DIRECTION ( 'NONE',  ( -1.000000000000000000, -0.000000000000000000, -0.000000000000000000 ) ) ;
#17909 = ORIENTED_EDGE ( 'NONE', *, *, #8034, .T. ) ;
#17910 = CARTESIAN_POINT ( 'NONE',  ( 7.500000000000000888, -0.7512838658081439913, 1.423015351387224570E-15 ) ) ;
#17911 = ORIENTED_EDGE ( 'NONE', *, *, #12322, .T. ) ;
#17912 = AXIS2_PLACEMENT_3D ( 'NONE', #12165, #22751, #21181 ) ;
#17913 = CARTESIAN_POINT ( 'NONE',  ( 0.000000000000000000, 0.000000000000000000, -150.0000000000000000 ) ) ;
#17914 = DIRECTION ( 'NONE',  ( 0.000000000000000000, 0.000000000000000000, 1.000000000000000000 ) ) ;
#17915 = ITEM_DEFINED_TRANSFORMATION ( 'NONE', 'NONE', #17748,  #11210 ) ;
#17916 = VERTEX_POINT ( 'NONE', #19835 ) ;
#17917 = DIRECTION ( 'NONE',  ( 1.776356839400250465E-15, 1.000000000000000000, -3.392348130799088816E-15 ) ) ;
#17918 = ORIENTED_EDGE ( 'NONE', *, *, #11862, .F. ) ;
#17919 = DIRECTION ( 'NONE',  ( 0.000000000000000000, 0.000000000000000000, 1.000000000000000000 ) ) ;
#17920 = CIRCLE ( 'NONE', #7497, 2.649999999999985700 ) ;
#17921 = DIRECTION ( 'NONE',  ( -0.000000000000000000, -1.000000000000000000, -0.000000000000000000 ) ) ;
#17922 = VERTEX_POINT ( 'NONE', #3285 ) ;
#17923 = DIRECTION ( 'NONE',  ( 0.000000000000000000, 0.000000000000000000, 1.000000000000000000 ) ) ;
#17924 = DIRECTION ( 'NONE',  ( 0.000000000000000000, 0.000000000000000000, -1.000000000000000000 ) ) ;
#17925=STYLED_ITEM('',(#23913),#4413);
#17926 = FACE_OUTER_BOUND ( 'NONE', #17772, .T. ) ;
#17927 = CIRCLE ( 'NONE', #18676, 2.499999999999946709 ) ;
#17928 = DIRECTION ( 'NONE',  ( 0.000000000000000000, -1.177509268541832635E-16, 1.000000000000000000 ) ) ;
#17929 = CARTESIAN_POINT ( 'NONE',  ( 105.0000000000000000, -19.99999999999998934, 3.000000000000001332 ) ) ;
#17930 = CARTESIAN_POINT ( 'NONE',  ( 0.000000000000000000, 0.000000000000000000, -90.00000000000000000 ) ) ;
#17931 = PLANE ( 'NONE',  #14176 ) ;
#17932 = VERTEX_POINT ( 'NONE', #12874 ) ;
#17933 = EDGE_CURVE ( 'NONE', #15087, #12421, #13435, .T. ) ;
#17934 = DIRECTION ( 'NONE',  ( -0.000000000000000000, -0.000000000000000000, 1.000000000000000000 ) ) ;
#17935 = CARTESIAN_POINT ( 'NONE',  ( 2.499999999999999112, -7.216878364870334295, -7.063244554130005959 ) ) ;
#17936 = ORIENTED_EDGE ( 'NONE', *, *, #6095, .F. ) ;
#17937 = ORIENTED_EDGE ( 'NONE', *, *, #4761, .F. ) ;
#17938 = AXIS2_PLACEMENT_3D ( 'NONE', #13796, #21120, #4577 ) ;
#17939 = ADVANCED_FACE ( 'NONE', ( #23457 ), #14426, .F. ) ;
#17940 = CARTESIAN_POINT ( 'NONE',  ( -155.0000000000000284, -1000.000000000000000, 90.00000000000000000 ) ) ;
#17941 = CARTESIAN_POINT ( 'NONE',  ( 45.00000000000004974, -56.79999999999965610, 102.3500000000002217 ) ) ;
#17942 = CARTESIAN_POINT ( 'NONE',  ( -280.5679143846944044, 269.9132285165672442, 145.2488155364689248 ) ) ;
#17943 = AXIS2_PLACEMENT_3D ( 'NONE', #77, #193, #11439 ) ;
#17944 = DIRECTION ( 'NONE',  ( 0.000000000000000000, 0.000000000000000000, 1.000000000000000000 ) ) ;
#17945 = DIRECTION ( 'NONE',  ( -1.000000000000000000, -0.000000000000000000, -0.000000000000000000 ) ) ;
#17946 = ORIENTED_EDGE ( 'NONE', *, *, #8013, .T. ) ;
#17947 = DIRECTION ( 'NONE',  ( 1.000000000000000000, 0.000000000000000000, 0.000000000000000000 ) ) ;
#17948 = EDGE_LOOP ( 'NONE', ( #6298, #4193, #17777, #5013 ) ) ;
#17949 = DIRECTION ( 'NONE',  ( -1.000000000000000000, -0.000000000000000000, -0.000000000000000000 ) ) ;
#17950 = FACE_BOUND ( 'NONE', #22610, .T. ) ;
#17951 = AXIS2_PLACEMENT_3D ( 'NONE', #4074, #11484, #9671 ) ;
#17952 = DIRECTION ( 'NONE',  ( 0.000000000000000000, 0.000000000000000000, 1.000000000000000000 ) ) ;
#17953 = ORIENTED_EDGE ( 'NONE', *, *, #12125, .T. ) ;
#17954 = CARTESIAN_POINT ( 'NONE',  ( -20.63749999999999574, 0.000000000000000000, -25.00000000000000000 ) ) ;
#17955 = FACE_OUTER_BOUND ( 'NONE', #3828, .T. ) ;
#17956 = CARTESIAN_POINT ( 'NONE',  ( -5.000000000000000000, -5.773502691896264416, -7.063244554130003294 ) ) ;
#17957 = DIRECTION ( 'NONE',  ( -6.753181414994864868E-15, 6.753181414994864868E-15, -1.000000000000000000 ) ) ;
#17958 = CARTESIAN_POINT ( 'NONE',  ( 2.500000000000000000, 1.178949249685213863, -2.042000000000001148 ) ) ;
#17959 = DIRECTION ( 'NONE',  ( -1.000000000000000000, 3.495664435217746987E-15, 0.000000000000000000 ) ) ;
#17960 = EDGE_CURVE ( 'NONE', #12056, #6599, #8005, .T. ) ;
#17961 = CARTESIAN_POINT ( 'NONE',  ( 5.000000000000000888, 4.250000000000000000, 0.000000000000000000 ) ) ;
#17962 = AXIS2_PLACEMENT_3D ( 'NONE', #4881, #19597, #14435 ) ;
#17963 = VECTOR ( 'NONE', #13205, 1000.000000000000000 ) ;
#17964 = ORIENTED_EDGE ( 'NONE', *, *, #15584, .F. ) ;
#17965 = EDGE_LOOP ( 'NONE', ( #16746, #2862, #22199, #10107 ) ) ;
#17966 = DIRECTION ( 'NONE',  ( -1.000000000000000000, 0.000000000000000000, 0.000000000000000000 ) ) ;
#17967 = DIRECTION ( 'NONE',  ( -1.000000000000000000, 1.408839003528726857E-14, 6.982962677686266711E-15 ) ) ;
#17968 = ORIENTED_EDGE ( 'NONE', *, *, #12955, .T. ) ;
#17969 = DIRECTION ( 'NONE',  ( -1.000000000000000000, 0.000000000000000000, 0.000000000000000000 ) ) ;
#17970 = FACE_BOUND ( 'NONE', #6265, .T. ) ;
#17971 = EDGE_CURVE ( 'NONE', #8260, #4200, #3402, .T. ) ;
#17972 = ORIENTED_EDGE ( 'NONE', *, *, #23208, .T. ) ;
#17973 = CARTESIAN_POINT ( 'NONE',  ( -287.4000000000014552, -127.0000000000000568, 146.4928932188134638 ) ) ;
#17974 = CARTESIAN_POINT ( 'NONE',  ( -2.670017925772866452, 9.709364418299751165, 200.0000120000000265 ) ) ;
#17975 = CIRCLE ( 'NONE', #7550, 35.00000000000000711 ) ;
#17976 = ORIENTED_EDGE ( 'NONE', *, *, #18746, .T. ) ;
#17977 = DIRECTION ( 'NONE',  ( -1.000000000000000000, 1.224646799147352714E-16, 0.000000000000000000 ) ) ;
#17978 = EDGE_CURVE ( 'NONE', #3965, #8982, #20178, .T. ) ;
#17979 = VECTOR ( 'NONE', #523, 1000.000000000000000 ) ;
#17980 = ORIENTED_EDGE ( 'NONE', *, *, #14052, .F. ) ;
#17981 = CARTESIAN_POINT ( 'NONE',  ( -288.2000000000013529, -89.99999999999896261, -42.98333333333330586 ) ) ;
#17982 = DIRECTION ( 'NONE',  ( -1.000000000000000000, -0.000000000000000000, -0.000000000000000000 ) ) ;
#17983 = ORIENTED_EDGE ( 'NONE', *, *, #10154, .F. ) ;
#17984 = ORIENTED_EDGE ( 'NONE', *, *, #22640, .T. ) ;
#17985 = CARTESIAN_POINT ( 'NONE',  ( 45.00000000000004974, -52.79999999999965610, 105.0000000000001990 ) ) ;
#17986 = PRODUCT_DEFINITION_SHAPE ( 'NONE', 'NONE',  #23852 ) ;
#17987 = CARTESIAN_POINT ( 'NONE',  ( -277.2000000000009550, 30.00000000000097344, -105.0000000000000142 ) ) ;
#17988 = CARTESIAN_POINT ( 'NONE',  ( -110.0000000000000000, 75.00000000000001421, 3.000000000000000000 ) ) ;
#17989 = CIRCLE ( 'NONE', #11062, 2.649999999999999467 ) ;
#17990 = DIRECTION ( 'NONE',  ( 0.000000000000000000, 0.000000000000000000, -1.000000000000000000 ) ) ;
#17991 = FACE_OUTER_BOUND ( 'NONE', #2528, .T. ) ;
#17992 = ORIENTED_EDGE ( 'NONE', *, *, #7406, .T. ) ;
#17993 = DIRECTION ( 'NONE',  ( -1.000000000000000000, 1.408839003528726857E-14, 6.982962677686266711E-15 ) ) ;
#17994 =( LENGTH_UNIT ( ) NAMED_UNIT ( * ) SI_UNIT ( .MILLI., .METRE. ) );
#17995 = ORIENTED_EDGE ( 'NONE', *, *, #22344, .F. ) ;
#17996 = EDGE_CURVE ( 'NONE', #14601, #13599, #13075, .T. ) ;
#17997 = ADVANCED_FACE ( 'NONE', ( #12766 ), #18255, .F. ) ;
#17998 = DIRECTION ( 'NONE',  ( 1.000000000000000000, 0.000000000000000000, 0.000000000000000000 ) ) ;
#17999 = CARTESIAN_POINT ( 'NONE',  ( 124.4701338314437891, -1092.369831568442805, 27.50000000000646239 ) ) ;
#18000 = ORIENTED_EDGE ( 'NONE', *, *, #23579, .F. ) ;
#18001 = AXIS2_PLACEMENT_3D ( 'NONE', #23661, #5198, #19803 ) ;
#18002 = CARTESIAN_POINT ( 'NONE',  ( 3.080866544135574259, 6.881514909250401324, -7.026396753507782478 ) ) ;
#18003 = EDGE_CURVE ( 'NONE', #6854, #11293, #1087, .T. ) ;
#18004 = DIRECTION ( 'NONE',  ( 1.000000000000000000, 0.000000000000000000, 0.000000000000000000 ) ) ;
#18005 = EDGE_CURVE ( 'NONE', #2744, #23060, #690, .T. ) ;
#18006 = ORIENTED_EDGE ( 'NONE', *, *, #6340, .F. ) ;
#18007 = CARTESIAN_POINT ( 'NONE',  ( 93.00000000000000000, -149.9999999999996874, 129.9038105676659711 ) ) ;
#18008 = ORIENTED_EDGE ( 'NONE', *, *, #19298, .T. ) ;
#18009 = EDGE_CURVE ( 'NONE', #18517, #19415, #9964, .T. ) ;
#18010 = DIRECTION ( 'NONE',  ( 0.000000000000000000, -0.4999999999999979461, 0.8660254037844397068 ) ) ;
#18011 = SURFACE_STYLE_FILL_AREA ( #1455 ) ;
#18012 = EDGE_CURVE ( 'NONE', #8135, #11056, #8022, .T. ) ;
#18013 = CIRCLE ( 'NONE', #1018, 0.4000000000000001887 ) ;
#18014 = CARTESIAN_POINT ( 'NONE',  ( 34.75000000000005684, 100.0000000000000000, 150.2000000000009550 ) ) ;
#18015 = DIRECTION ( 'NONE',  ( 1.000000000000000000, 0.000000000000000000, 0.000000000000000000 ) ) ;
#18016 = FACE_OUTER_BOUND ( 'NONE', #11825, .T. ) ;
#18017 = VERTEX_POINT ( 'NONE', #7506 ) ;
#18018 = DIRECTION ( 'NONE',  ( 0.000000000000000000, 0.000000000000000000, 1.000000000000000000 ) ) ;
#18019 = VECTOR ( 'NONE', #4575, 1000.000000000000000 ) ;
#18021 = VERTEX_POINT ( 'NONE', #20910 ) ;
#18020 = ORIENTED_EDGE ( 'NONE', *, *, #15510, .F. ) ;
#18022 = CARTESIAN_POINT ( 'NONE',  ( -8.339331917296304295E-16, -1000.000000000000000, 142.0000000000000284 ) ) ;
#18023 = DIRECTION ( 'NONE',  ( -0.000000000000000000, -0.000000000000000000, 1.000000000000000000 ) ) ;
#18024 = DIRECTION ( 'NONE',  ( 0.000000000000000000, 0.000000000000000000, 1.000000000000000000 ) ) ;
#18025 = CARTESIAN_POINT ( 'NONE',  ( 30.00000000000000000, 0.000000000000000000, -6.938893903907228378E-15 ) ) ;
#18026 = CARTESIAN_POINT ( 'NONE',  ( -45.00000000000000000, 269.9999999999999432, 5.249999999999973355 ) ) ;
#18027 = EDGE_CURVE ( 'NONE', #45, #2904, #15140, .T. ) ;
#18028 = ORIENTED_EDGE ( 'NONE', *, *, #9457, .T. ) ;
#18029 = EDGE_CURVE ( 'NONE', #6740, #21770, #3755, .T. ) ;
#18030 = AXIS2_PLACEMENT_3D ( 'NONE', #4566, #2757, #23161 ) ;
#18031 = DIRECTION ( 'NONE',  ( -0.000000000000000000, -0.000000000000000000, 1.000000000000000000 ) ) ;
#18032 = ORIENTED_EDGE ( 'NONE', *, *, #13607, .F. ) ;
#18033 = EDGE_CURVE ( 'NONE', #22609, #4934, #22716, .T. ) ;
#18034 = AXIS2_PLACEMENT_3D ( 'NONE', #8025, #15405, #4144 ) ;
#18035 = PLANE ( 'NONE',  #8858 ) ;
#18036 = DIRECTION ( 'NONE',  ( 1.000000000000000000, 0.000000000000000000, 0.000000000000000000 ) ) ;
#18037 = VECTOR ( 'NONE', #6997, 1000.000000000000000 ) ;
#18038 = EDGE_LOOP ( 'NONE', ( #7342, #1410, #9975, #4088 ) ) ;
#18039 = CIRCLE ( 'NONE', #1065, 2.200000000000028155 ) ;
#18040 = ORIENTED_EDGE ( 'NONE', *, *, #1464, .F. ) ;
#18041 = ADVANCED_FACE ( 'NONE', ( #2314 ), #6188, .T. ) ;
#18042 = LINE ( 'NONE', #14089, #19114 ) ;
#18043 = EDGE_LOOP ( 'NONE', ( #3516, #2790, #10436, #22346 ) ) ;
#18044 = EDGE_CURVE ( 'NONE', #20235, #19527, #9181, .T. ) ;
#18045 = CARTESIAN_POINT ( 'NONE',  ( 285.1999999999999318, 267.7999999999999545, -146.4928932188134070 ) ) ;
#18046 = CARTESIAN_POINT ( 'NONE',  ( 133.8630869304073485, 78.13886732029855864, 28.46749050845387075 ) ) ;
#18047 = CARTESIAN_POINT ( 'NONE',  ( 0.2727178028658734932, 0.000000000000000000, 21.02499999999999503 ) ) ;
#18048 = PLANE ( 'NONE',  #4400 ) ;
#18049 = PLANE ( 'NONE',  #15035 ) ;
#18050 = FACE_OUTER_BOUND ( 'NONE', #9685, .T. ) ;
#18051 = VECTOR ( 'NONE', #4894, 1000.000000000000000 ) ;
#18052 = ORIENTED_EDGE ( 'NONE', *, *, #1664, .T. ) ;
#18053 = AXIS2_PLACEMENT_3D ( 'NONE', #6846, #10736, #1407 ) ;
#18054 = CARTESIAN_POINT ( 'NONE',  ( -7.499999999999999112, 1.443375672974061219, -7.063244554130000630 ) ) ;
#18055 = CARTESIAN_POINT ( 'NONE',  ( 125.6044290879524965, 79.19280534549594108, 30.00000000000641620 ) ) ;
#18056 = VECTOR ( 'NONE', #16151, 1000.000000000000000 ) ;
#18057 = EDGE_LOOP ( 'NONE', ( #11490, #4857 ) ) ;
#18058 = VECTOR ( 'NONE', #15786, 1000.000000000000000 ) ;
#18059 = LINE ( 'NONE', #1507, #18866 ) ;
#18060 = DIRECTION ( 'NONE',  ( -3.469446951953614682E-16, 1.000000000000000000, -3.483493295888648978E-15 ) ) ;
#18061 = CARTESIAN_POINT ( 'NONE',  ( -283.1956429438696432, 271.9582675804705332, 145.6220388411722695 ) ) ;
#18062 = DIRECTION ( 'NONE',  ( 0.000000000000000000, 0.000000000000000000, 1.000000000000000000 ) ) ;
#18063 = CARTESIAN_POINT ( 'NONE',  ( 5.000000000000004441, 0.000000000000000000, 0.000000000000000000 ) ) ;
#18064 = EDGE_LOOP ( 'NONE', ( #14471, #4719, #8586, #10597 ) ) ;
#18065 = LINE ( 'NONE', #12556, #1143 ) ;
#18066 = ORIENTED_EDGE ( 'NONE', *, *, #22824, .F. ) ;
#18067 = DIRECTION ( 'NONE',  ( 0.000000000000000000, 0.000000000000000000, 1.000000000000000000 ) ) ;
#18068 = DIRECTION ( 'NONE',  ( 0.000000000000000000, -1.000000000000000000, -1.110223024625156540E-16 ) ) ;
#18069 = ADVANCED_FACE ( 'NONE', ( #20539 ), #20659, .F. ) ;
#18070 = ADVANCED_FACE ( 'NONE', ( #11404 ), #22659, .F. ) ;
#18071 = VECTOR ( 'NONE', #4126, 1000.000000000000000 ) ;
#18072 = ORIENTED_EDGE ( 'NONE', *, *, #4728, .T. ) ;
#18073 = CARTESIAN_POINT ( 'NONE',  ( -6.901579824520442941, 4.675625068323816080, -0.7022220667781327030 ) ) ;
#18074 = AXIS2_PLACEMENT_3D ( 'NONE', #13962, #15737, #2441 ) ;
#18075 = LINE ( 'NONE', #1530, #21493 ) ;
#18076 = EDGE_CURVE ( 'NONE', #2426, #1928, #6863, .T. ) ;
#18077 = CARTESIAN_POINT ( 'NONE',  ( -7.500000000000000000, 4.330127018922191873, -0.9999999999999970024 ) ) ;
#18078 = CARTESIAN_POINT ( 'NONE',  ( -79.99999999999995737, -138.0000000000000284, 3.000000000000000000 ) ) ;
#18079 = CARTESIAN_POINT ( 'NONE',  ( 26.98333333333330231, -89.99999999999998579, 0.000000000000000000 ) ) ;
#18080 = FACE_OUTER_BOUND ( 'NONE', #18966, .T. ) ;
#18081 = AXIS2_PLACEMENT_3D ( 'NONE', #8916, #16271, #23616 ) ;
#18082 = CARTESIAN_POINT ( 'NONE',  ( 23.72315261474502179, 8.055391459054641601, 145.0000119999999697 ) ) ;
#18083 = SHAPE_REPRESENTATION ( 'socket head cap screw_iso_ISO 4762 M5 x 12 - 12N', ( #11210 ), #3838 ) ;
#18084 = ORIENTED_EDGE ( 'NONE', *, *, #19441, .T. ) ;
#18085 = ORIENTED_EDGE ( 'NONE', *, *, #19386, .T. ) ;
#18086 = DIRECTION ( 'NONE',  ( 0.000000000000000000, 0.000000000000000000, 1.000000000000000000 ) ) ;
#18087 = CARTESIAN_POINT ( 'NONE',  ( -281.4928932188135491, -127.0000000000000568, 150.2000000000013813 ) ) ;
#18088 = EDGE_LOOP ( 'NONE', ( #12256, #19749, #3844, #18326 ) ) ;
#18089 = B_SPLINE_SURFACE_WITH_KNOTS ( 'NONE', 1, 3, ( 
 ( #9942, #22833, #858, #11776, #4615, #17300, #2554, #21275, #8238, #19328 ),
 ( #6300, #15861, #15727, #13711, #21030, #8350, #749, #8133, #17178, #6547 ),
 ( #6418, #4491, #971, #12138, #2788, #4253, #15504, #4368, #23068, #2431 ),
 ( #19436, #11898, #11662, #19206, #15616, #17635, #19086, #22945, #13823, #21149 ) ),
 .UNSPECIFIED., .F., .F., .F.,
 ( 2, 1, 1, 2 ),
 ( 4, 2, 2, 2, 4 ),
 ( -0.01000000000000000021, 0.000000000000000000, 1.000000000000000000, 1.010099999999999998 ),
 ( 0.000000000000000000, 0.2500000000000000000, 0.5000000000000000000, 0.7500000000000000000, 1.000000000000000000 ),
 .UNSPECIFIED. ) ;
#18090 = CIRCLE ( 'NONE', #18467, 5.400000000000002132 ) ;
#18091 = CARTESIAN_POINT ( 'NONE',  ( 2.500000000000002220, -2.357898499370430834, 3.469446951953614189E-15 ) ) ;
#18092 = FACE_BOUND ( 'NONE', #10523, .T. ) ;
#18093 = CIRCLE ( 'NONE', #20377, 5.249999999999949374 ) ;
#18094 = AXIS2_PLACEMENT_3D ( 'NONE', #17851, #1297, #8679 ) ;
#18095 = VECTOR ( 'NONE', #8309, 1000.000000000000000 ) ;
#18096 = VERTEX_POINT ( 'NONE', #18843 ) ;
#18097 = CARTESIAN_POINT ( 'NONE',  ( 280.1244294735508333, 272.9999999999999432, 145.6807971656549228 ) ) ;
#18098 = AXIS2_PLACEMENT_3D ( 'NONE', #18504, #3890, #5702 ) ;
#18099 = VECTOR ( 'NONE', #22093, 1000.000000000000000 ) ;
#18100 = CARTESIAN_POINT ( 'NONE',  ( 0.000000000000000000, 0.000000000000000000, 100.0000000000000000 ) ) ;
#18101 = ORIENTED_EDGE ( 'NONE', *, *, #14119, .F. ) ;
#18102 = DIRECTION ( 'NONE',  ( 1.000000000000000000, 0.000000000000000000, 0.000000000000000000 ) ) ;
#18103 = ORIENTED_EDGE ( 'NONE', *, *, #22133, .F. ) ;
#18104 = CARTESIAN_POINT ( 'NONE',  ( -44.99999999999997868, -56.79999999999937899, 140.0000000000001421 ) ) ;
#18105 = CYLINDRICAL_SURFACE ( 'NONE', #22559, 2.649999999999971934 ) ;
#18106 = DIRECTION ( 'NONE',  ( -1.000000000000000000, 1.408839003528726857E-14, 6.982962677686266711E-15 ) ) ;
#18107 = ORIENTED_EDGE ( 'NONE', *, *, #10106, .T. ) ;
#18108 = ORIENTED_EDGE ( 'NONE', *, *, #16579, .F. ) ;
#18109 = CARTESIAN_POINT ( 'NONE',  ( 283.2140793454687469, 271.9822575857424454, -145.6220388411722126 ) ) ;
#18110 = ADVANCED_FACE ( 'NONE', ( #15257, #19325, #10293, #8234, #3014, #15725, #15859, #4841, #10429 ), #2786, .T. ) ;
#18111 = PRESENTATION_LAYER_ASSIGNMENT (  '', '', ( #3437 ) ) ;
#18112 = DIRECTION ( 'NONE',  ( 0.000000000000000000, 0.8660254037844380415, -0.5000000000000012212 ) ) ;
#18113 = VECTOR ( 'NONE', #21531, 1000.000000000000000 ) ;
#18114 = VECTOR ( 'NONE', #12751, 999.9999999999998863 ) ;
#18115 = AXIS2_PLACEMENT_3D ( 'NONE', #22869, #9983, #8173 ) ;
#18116 = AXIS2_PLACEMENT_3D ( 'NONE', #14569, #9130, #9490 ) ;
#18117 = FACE_BOUND ( 'NONE', #2424, .T. ) ;
#18118 = AXIS2_PLACEMENT_3D ( 'NONE', #23101, #17914, #21412 ) ;
#18119 = VECTOR ( 'NONE', #19521, 1000.000000000000000 ) ;
#18120 = EDGE_LOOP ( 'NONE', ( #17805, #23286, #16407, #1537 ) ) ;
#18121 = CARTESIAN_POINT ( 'NONE',  ( 2.699999999999995737, 2.486033002269127373E-15, 20.30000000000000071 ) ) ;
#18122 = CARTESIAN_POINT ( 'NONE',  ( -64.99999999999998579, -56.79999999999943583, 125.0000000000001705 ) ) ;
#18123 = DIRECTION ( 'NONE',  ( -1.000000000000000000, -3.491481338843133355E-15, 0.000000000000000000 ) ) ;
#18124 = VERTEX_POINT ( 'NONE', #12250 ) ;
#18125 = DIRECTION ( 'NONE',  ( 1.000000000000000000, -0.000000000000000000, -0.000000000000000000 ) ) ;
#18126 =( GEOMETRIC_REPRESENTATION_CONTEXT ( 3 ) GLOBAL_UNCERTAINTY_ASSIGNED_CONTEXT ( ( #9655 ) ) GLOBAL_UNIT_ASSIGNED_CONTEXT ( ( #11540, #5954, #17072 ) ) REPRESENTATION_CONTEXT ( 'NONE', 'WORKASPACE' ) );
#18127 = VECTOR ( 'NONE', #3519, 1000.000000000000000 ) ;
#18128 = VECTOR ( 'NONE', #4585, 1000.000000000000000 ) ;
#18129 = CIRCLE ( 'NONE', #2715, 20.00000000000000000 ) ;
#18130 = ORIENTED_EDGE ( 'NONE', *, *, #14537, .T. ) ;
#18131 = PLANE ( 'NONE',  #23701 ) ;
#18132 = ORIENTED_EDGE ( 'NONE', *, *, #18779, .F. ) ;
#18133 = CIRCLE ( 'NONE', #21156, 4.250000000000000000 ) ;
#18134 = EDGE_CURVE ( 'NONE', #422, #11691, #22942, .T. ) ;
#18135 = DIRECTION ( 'NONE',  ( 0.000000000000000000, -1.000000000000000000, -4.183096374613631247E-18 ) ) ;
#18136 = CARTESIAN_POINT ( 'NONE',  ( -281.3673618604588000, 268.0905802150185195, 147.2000000000000171 ) ) ;
#18137 = EDGE_CURVE ( 'NONE', #14233, #13071, #23709, .T. ) ;
#18138 = EDGE_CURVE ( 'NONE', #4268, #17746, #8318, .T. ) ;
#18139 = DIRECTION ( 'NONE',  ( -1.000000000000000000, -0.000000000000000000, -0.000000000000000000 ) ) ;
#18140 = CARTESIAN_POINT ( 'NONE',  ( 125.3835310783082093, -1091.126227143374990, -31.99040335529153367 ) ) ;
#18141 = CARTESIAN_POINT ( 'NONE',  ( 5.000000000000000000, 2.342598717236902939, -4.057500000000001883 ) ) ;
#18142 = ORIENTED_EDGE ( 'NONE', *, *, #1862, .F. ) ;
#18143 = AXIS2_PLACEMENT_3D ( 'NONE', #10650, #15948, #21364 ) ;
#18144 = DIRECTION ( 'NONE',  ( 0.000000000000000000, 0.000000000000000000, -1.000000000000000000 ) ) ;
#18145 = EDGE_CURVE ( 'NONE', #7169, #3375, #213, .T. ) ;
#18146 = AXIS2_PLACEMENT_3D ( 'NONE', #1191, #19075, #9932 ) ;
#18147 = CIRCLE ( 'NONE', #19291, 5.249999999999956479 ) ;
#18149 = VERTEX_POINT ( 'NONE', #8347 ) ;
#18148 = VERTEX_POINT ( 'NONE', #17633 ) ;
#18150 = DIRECTION ( 'NONE',  ( -3.469446951953613794E-15, 3.469446951953612611E-15, 1.000000000000000000 ) ) ;
#18151 = FACE_OUTER_BOUND ( 'NONE', #1070, .T. ) ;
#18152 = CARTESIAN_POINT ( 'NONE',  ( 2.500000000000000000, -1.178949249685213863, 2.042000000000002924 ) ) ;
#18153 = ORIENTED_EDGE ( 'NONE', *, *, #12476, .T. ) ;
#18154 = DIRECTION ( 'NONE',  ( 0.000000000000000000, 0.000000000000000000, -1.000000000000000000 ) ) ;
#18155 = CARTESIAN_POINT ( 'NONE',  ( -194.7500000000000000, -204.4690652294800657, 32.50000000000675726 ) ) ;
#18156 = ORIENTED_EDGE ( 'NONE', *, *, #23582, .T. ) ;
#18157 = DIRECTION ( 'NONE',  ( -0.7232617928448825673, 0.6905739489807055653, 0.000000000000000000 ) ) ;
#18158 = DIRECTION ( 'NONE',  ( 0.000000000000000000, 0.000000000000000000, 1.000000000000000000 ) ) ;
#18159 = DIRECTION ( 'NONE',  ( -1.110223024625157172E-14, 0.000000000000000000, -1.000000000000000000 ) ) ;
#18160 = VERTEX_POINT ( 'NONE', #13819 ) ;
#18161 = VERTEX_POINT ( 'NONE', #14053 ) ;
#18162 = DIRECTION ( 'NONE',  ( -0.000000000000000000, -0.000000000000000000, 1.000000000000000000 ) ) ;
#18163 = EDGE_LOOP ( 'NONE', ( #18175, #19493, #9151, #16810 ) ) ;
#18164 = FILL_AREA_STYLE_COLOUR ( '', #8237 ) ;
#18165 = CARTESIAN_POINT ( 'NONE',  ( 134.1263161626745557, 77.68610759098336871, 30.16266818053253118 ) ) ;
#18166 = CARTESIAN_POINT ( 'NONE',  ( 89.00000000000000000, -149.9999999999996874, 129.9038105676659711 ) ) ;
#18167 = CARTESIAN_POINT ( 'NONE',  ( -37.65000000000000568, 90.00000000000001421, 3.000000000000001332 ) ) ;
#18168 = FACE_OUTER_BOUND ( 'NONE', #14291, .T. ) ;
#18169 =( NAMED_UNIT ( * ) PLANE_ANGLE_UNIT ( ) SI_UNIT ( $, .RADIAN. ) );
#18170 = EDGE_CURVE ( 'NONE', #11764, #4268, #17517, .T. ) ;
#18171 = ADVANCED_FACE ( 'NONE', ( #13709, #2889 ), #21145, .T. ) ;
#18172 = ORIENTED_EDGE ( 'NONE', *, *, #11700, .F. ) ;
#18173 = CARTESIAN_POINT ( 'NONE',  ( -7.500000000000000000, -4.330127018922199866, -1.000000000000000888 ) ) ;
#18174 = FACE_OUTER_BOUND ( 'NONE', #22682, .T. ) ;
#18175 = ORIENTED_EDGE ( 'NONE', *, *, #790, .T. ) ;
#18176 = EDGE_CURVE ( 'NONE', #880, #20274, #7919, .T. ) ;
#18177 = CARTESIAN_POINT ( 'NONE',  ( 280.6842353883613441, 269.4574776399289249, -146.4538215477170127 ) ) ;
#18178 = CARTESIAN_POINT ( 'NONE',  ( 110.0000000000000000, -74.99999999999998579, 3.000000000000000000 ) ) ;
#18179 = EDGE_CURVE ( 'NONE', #1963, #6583, #15502, .T. ) ;
#18180 = EDGE_CURVE ( 'NONE', #18832, #2992, #21027, .T. ) ;
#18181 = DIRECTION ( 'NONE',  ( 0.000000000000000000, 0.000000000000000000, 1.000000000000000000 ) ) ;
#18182 = DIRECTION ( 'NONE',  ( 0.000000000000000000, 0.000000000000000000, -1.000000000000000000 ) ) ;
#18183 = CARTESIAN_POINT ( 'NONE',  ( 280.8706349181168775, 270.9682701916305518, -149.1268706878665284 ) ) ;
#18184 = VERTEX_POINT ( 'NONE', #856 ) ;
#18185 = DIRECTION ( 'NONE',  ( -0.000000000000000000, -1.177509268541832635E-16, 1.000000000000000000 ) ) ;
#18186 = EDGE_LOOP ( 'NONE', ( #22083, #242, #7955, #11737 ) ) ;
#18187 = CYLINDRICAL_SURFACE ( 'NONE', #11442, 5.199999999999982414 ) ;
#18188 = DIRECTION ( 'NONE',  ( -0.000000000000000000, 1.000000000000000000, 0.000000000000000000 ) ) ;
#18189 = CARTESIAN_POINT ( 'NONE',  ( -45.00000000000000000, 269.9999999999999432, 5.249999999999973355 ) ) ;
#18190 = EDGE_LOOP ( 'NONE', ( #13626, #21256 ) ) ;
#18191 = SURFACE_STYLE_FILL_AREA ( #18536 ) ;
#18192 = DIRECTION ( 'NONE',  ( -1.000000000000000000, -0.000000000000000000, -0.000000000000000000 ) ) ;
#18193 = CARTESIAN_POINT ( 'NONE',  ( -3.750000000000004885, 6.495190528383289141, 0.000000000000000000 ) ) ;
#18194 = CARTESIAN_POINT ( 'NONE',  ( -146.4450000000005332, -494.4690652294800657, -32.49999999999356248 ) ) ;
#18195 = DIRECTION ( 'NONE',  ( 1.000000000000000000, 0.000000000000000000, 0.000000000000000000 ) ) ;
#18196 = CYLINDRICAL_SURFACE ( 'NONE', #12416, 2.649999999999971934 ) ;
#18197 = CARTESIAN_POINT ( 'NONE',  ( 90.00000000000000000, 75.00000000000000000, 0.000000000000000000 ) ) ;
#18198 = ORIENTED_EDGE ( 'NONE', *, *, #21843, .T. ) ;
#18199 = EDGE_LOOP ( 'NONE', ( #11498, #8644 ) ) ;
#18200 = FACE_OUTER_BOUND ( 'NONE', #9837, .T. ) ;
#18201 = ORIENTED_EDGE ( 'NONE', *, *, #13089, .T. ) ;
#18202 = CARTESIAN_POINT ( 'NONE',  ( -194.7500000000004547, -204.4690652294793836, -27.49999999999322498 ) ) ;
#18203 = CARTESIAN_POINT ( 'NONE',  ( -0.3470952277635217520, -8.860649561028104415, -7.493596212620245112 ) ) ;
#18204 = ADVANCED_FACE ( 'NONE', ( #6543 ), #19460, .T. ) ;
#18205 = EDGE_CURVE ( 'NONE', #10923, #20782, #968, .T. ) ;
#18206 = ADVANCED_FACE ( 'NONE', ( #11627 ), #20880, .T. ) ;
#18207 = ORIENTED_EDGE ( 'NONE', *, *, #12402, .T. ) ;
#18208 = CARTESIAN_POINT ( 'NONE',  ( 281.4928932188133217, 267.7999999999999545, 147.1696999999999775 ) ) ;
#18209 = CARTESIAN_POINT ( 'NONE',  ( 3.093157300003884558, 6.874418838041288282, 2.127746763502802452E-15 ) ) ;
#18210 = ORIENTED_EDGE ( 'NONE', *, *, #7592, .T. ) ;
#18211 = CARTESIAN_POINT ( 'NONE',  ( 100.0000000000000000, -1420.000000000000000, 124.9999999999998295 ) ) ;
#18212 = DIRECTION ( 'NONE',  ( -1.000000000000000000, 0.000000000000000000, 0.000000000000000000 ) ) ;
#18213 = ORIENTED_EDGE ( 'NONE', *, *, #3507, .F. ) ;
#18214 = DIRECTION ( 'NONE',  ( -1.000000000000000000, -0.000000000000000000, -0.000000000000000000 ) ) ;
#18215 = CARTESIAN_POINT ( 'NONE',  ( 0.000000000000000000, 0.000000000000000000, -147.2000000000008981 ) ) ;
#18216 = CYLINDRICAL_SURFACE ( 'NONE', #10587, 2.500000000000002220 ) ;
#18217 = ORIENTED_EDGE ( 'NONE', *, *, #19775, .F. ) ;
#18218 = ORIENTED_EDGE ( 'NONE', *, *, #15508, .F. ) ;
#18219 = CARTESIAN_POINT ( 'NONE',  ( 40.00000000000000000, 100.0000000000000000, -147.2000000000005571 ) ) ;
#18220 = VECTOR ( 'NONE', #7607, 1000.000000000000000 ) ;
#18221 = CARTESIAN_POINT ( 'NONE',  ( -40.00000000000000000, 100.0000000000000000, -160.2000000000005855 ) ) ;
#18222 = CARTESIAN_POINT ( 'NONE',  ( -127.0280029979305141, 88.81950979153471337, -31.99339931332765374 ) ) ;
#18223 = CARTESIAN_POINT ( 'NONE',  ( 0.000000000000000000, 0.000000000000000000, 22.50000000000000000 ) ) ;
#18224 = CARTESIAN_POINT ( 'NONE',  ( 80.00000000000001421, -59.79999999999913030, 250.0000000000000000 ) ) ;
#18225 = VERTEX_POINT ( 'NONE', #593 ) ;
#18226 = LINE ( 'NONE', #11261, #13039 ) ;
#18227 =( LENGTH_UNIT ( ) NAMED_UNIT ( * ) SI_UNIT ( .MILLI., .METRE. ) );
#18228 = DIRECTION ( 'NONE',  ( 5.551115123125785858E-15, 0.000000000000000000, -1.000000000000000000 ) ) ;
#18229 = CARTESIAN_POINT ( 'NONE',  ( -1.499999046620369203, 9.887721681869660273, 200.0000060000000133 ) ) ;
#18230 = ORIENTED_EDGE ( 'NONE', *, *, #13128, .T. ) ;
#18231 = CARTESIAN_POINT ( 'NONE',  ( 24.99999999999998579, 45.00100000000075084, 154.9999999999998579 ) ) ;
#18232 = ORIENTED_EDGE ( 'NONE', *, *, #12033, .F. ) ;
#18233 = LINE ( 'NONE', #124, #9067 ) ;
#18234 = EDGE_LOOP ( 'NONE', ( #18361, #18529 ) ) ;
#18235 = CARTESIAN_POINT ( 'NONE',  ( -282.2000000000006708, 90.00000000000102318, -35.00000000000001421 ) ) ;
#18236 = CARTESIAN_POINT ( 'NONE',  ( 19.87769063953884796, -1015.249744797204698, 145.0000119999999697 ) ) ;
#18237 = DIRECTION ( 'NONE',  ( 0.000000000000000000, -0.7071067811865485719, -0.7071067811865465735 ) ) ;
#18238 = AXIS2_PLACEMENT_3D ( 'NONE', #19607, #1013, #8392 ) ;
#18239 = CARTESIAN_POINT ( 'NONE',  ( 99.99999999999997158, 34.99999999999995026, -113.4834095219707848 ) ) ;
#18240 = CARTESIAN_POINT ( 'NONE',  ( -7.499999999999999112, 41.99999999999998579, 100.0000000000000000 ) ) ;
#18241 = ORIENTED_EDGE ( 'NONE', *, *, #19198, .T. ) ;
#18242 = CARTESIAN_POINT ( 'NONE',  ( 5.000000000000000000, -4.685197434473811207, 4.770489558936219510E-15 ) ) ;
#18243 =( NAMED_UNIT ( * ) PLANE_ANGLE_UNIT ( ) SI_UNIT ( $, .RADIAN. ) );
#18244 = ADVANCED_FACE ( 'NONE', ( #13426 ), #16402, .F. ) ;
#18246 = VERTEX_POINT ( 'NONE', #15471 ) ;
#18245 = ORIENTED_EDGE ( 'NONE', *, *, #17519, .T. ) ;
#18247 = CARTESIAN_POINT ( 'NONE',  ( 69.99999999999997158, -112.6666666666666856, 119.9999999999999716 ) ) ;
#18248 = CARTESIAN_POINT ( 'NONE',  ( -20.63749999999999574, 0.000000000000000000, 0.000000000000000000 ) ) ;
#18249 = CYLINDRICAL_SURFACE ( 'NONE', #695, 10.00000000000000000 ) ;
#18250 = VERTEX_POINT ( 'NONE', #7835 ) ;
#18251 = CIRCLE ( 'NONE', #5935, 2.199999999999979750 ) ;
#18252 = ADVANCED_FACE ( 'NONE', ( #18801 ), #20615, .T. ) ;
#18253 = CARTESIAN_POINT ( 'NONE',  ( -282.2000000000014666, -127.0000000000000568, 146.4928932188134638 ) ) ;
#18254 = ADVANCED_FACE ( 'NONE', ( #6268 ), #17136, .T. ) ;
#18255 = CYLINDRICAL_SURFACE ( 'NONE', #20338, 2.649999999999985700 ) ;
#18256 = VERTEX_POINT ( 'NONE', #4205 ) ;
#18257 = DIRECTION ( 'NONE',  ( 0.000000000000000000, -0.7071067811865465735, 0.7071067811865485719 ) ) ;
#18258 = CARTESIAN_POINT ( 'NONE',  ( 2.500000000000000000, 1.768423874527823791, 1.020999999999998353 ) ) ;
#18259 = EDGE_CURVE ( 'NONE', #9588, #4934, #19874, .T. ) ;
#18260 = ORIENTED_EDGE ( 'NONE', *, *, #21500, .T. ) ;
#18261 = ORIENTED_EDGE ( 'NONE', *, *, #8614, .T. ) ;
#18262 = CARTESIAN_POINT ( 'NONE',  ( 45.00000000000004974, -56.79999999999967031, 50.00000000000019895 ) ) ;
#18263 = ORIENTED_EDGE ( 'NONE', *, *, #1733, .F. ) ;
#18264 = CARTESIAN_POINT ( 'NONE',  ( 5.000000000000000000, 0.000000000000000000, 4.057500000000000107 ) ) ;
#18265 = DIRECTION ( 'NONE',  ( -0.000000000000000000, -0.000000000000000000, -1.000000000000000000 ) ) ;
#18266 = CARTESIAN_POINT ( 'NONE',  ( -285.2000000000006708, 90.00000000000102318, -37.64999999999999147 ) ) ;
#18267 = AXIS2_PLACEMENT_3D ( 'NONE', #8197, #22895, #17714 ) ;
#18268 = B_SPLINE_SURFACE_WITH_KNOTS ( 'NONE', 1, 3, ( 
 ( #9842, #2451, #15283, #5847, #13618, #15048, #13370, #13256, #7779, #20451 ),
 ( #22385, #22494, #2569, #20564, #770, #6211, #22614, #11796, #5962, #11679 ),
 ( #22249, #22743, #20681, #4138, #8152, #9724, #3905, #17199, #20928, #15401 ),
 ( #16962, #4015, #19110, #292, #11553, #11430, #5725, #17324, #4388, #13499 ) ),
 .UNSPECIFIED., .F., .F., .F.,
 ( 2, 1, 1, 2 ),
 ( 4, 2, 2, 2, 4 ),
 ( -0.01000000000000000021, 0.000000000000000000, 1.000000000000000000, 1.010099999999999998 ),
 ( 0.000000000000000000, 0.2500000000000000000, 0.5000000000000000000, 0.7500000000000000000, 1.000000000000000000 ),
 .UNSPECIFIED. ) ;
#18269 = AXIS2_PLACEMENT_3D ( 'NONE', #18078, #17840, #1287 ) ;
#18270 = CARTESIAN_POINT ( 'NONE',  ( -72.64999999999996305, -87.33333333333338544, 145.0000000000000000 ) ) ;
#18271 = CARTESIAN_POINT ( 'NONE',  ( -287.4000000000014552, -127.0000000000000568, 146.4928932188134638 ) ) ;
#18272 = FILL_AREA_STYLE_COLOUR ( '', #7717 ) ;
#18273 = ORIENTED_EDGE ( 'NONE', *, *, #16430, .F. ) ;
#18274 = LINE ( 'NONE', #7415, #9194 ) ;
#18275 = CARTESIAN_POINT ( 'NONE',  ( 0.000000000000000000, -132.2000000000000455, 177.2000000000014097 ) ) ;
#18276 = ORIENTED_EDGE ( 'NONE', *, *, #10516, .F. ) ;
#18277 = CARTESIAN_POINT ( 'NONE',  ( 280.4357197208658476, 269.7771302778488121, -145.9755403010746875 ) ) ;
#18278 = EDGE_CURVE ( 'NONE', #17134, #19974, #11859, .T. ) ;
#18279 = CARTESIAN_POINT ( 'NONE',  ( 155.0000000000000284, 2.775557561562891351E-16, 90.00000000000000000 ) ) ;
#18280 = CARTESIAN_POINT ( 'NONE',  ( -284.5436892194422285, 270.4188186979286002, 145.9952621458756425 ) ) ;
#18281 = AXIS2_PLACEMENT_3D ( 'NONE', #9495, #16735, #11083 ) ;
#18282 = CARTESIAN_POINT ( 'NONE',  ( 67.35000000000002274, -112.6666666666666714, 144.9999999999999716 ) ) ;
#18283 = CARTESIAN_POINT ( 'NONE',  ( 280.1247002395579102, 272.9663407402831581, -145.6822561791009321 ) ) ;
#18284 = EDGE_CURVE ( 'NONE', #16905, #9249, #20244, .T. ) ;
#18285 = VERTEX_POINT ( 'NONE', #702 ) ;
#18286 = CARTESIAN_POINT ( 'NONE',  ( -19.87769063953885507, -984.7502552027950742, 145.0000119999999697 ) ) ;
#18287 = ADVANCED_FACE ( 'NONE', ( #15107 ), #23334, .F. ) ;
#18288 = ORIENTED_EDGE ( 'NONE', *, *, #2476, .T. ) ;
#18289 = DIRECTION ( 'NONE',  ( 0.000000000000000000, 0.7071067811865485719, 0.7071067811865465735 ) ) ;
#18290 = SURFACE_STYLE_USAGE ( .BOTH. , #23617 ) ;
#18291 = ORIENTED_EDGE ( 'NONE', *, *, #17434, .F. ) ;
#18292 = CYLINDRICAL_SURFACE ( 'NONE', #17678, 2.649999999999971934 ) ;
#18293 = EDGE_CURVE ( 'NONE', #17025, #19104, #11365, .T. ) ;
#18294 = CARTESIAN_POINT ( 'NONE',  ( 123.4701789281957787, -1093.702342252440303, -28.11073331261971830 ) ) ;
#18295 = DIRECTION ( 'NONE',  ( -0.5877852522924773560, 0.8090169943749444537, 0.000000000000000000 ) ) ;
#18296 = CARTESIAN_POINT ( 'NONE',  ( 34.75000000000005684, 100.0000000000000000, -150.2000000000005571 ) ) ;
#18297 = PLANE ( 'NONE',  #13112 ) ;
#18298 = ADVANCED_FACE ( 'NONE', ( #19168 ), #11407, .T. ) ;
#18299 = CARTESIAN_POINT ( 'NONE',  ( 10.00000000000000178, 0.000000000000000000, 0.000000000000000000 ) ) ;
#18300 = CARTESIAN_POINT ( 'NONE',  ( -1.636246173744691390, 25.00000000000000355, 145.0000119999999697 ) ) ;
#18301 = ORIENTED_EDGE ( 'NONE', *, *, #14952, .F. ) ;
#18302 = ORIENTED_EDGE ( 'NONE', *, *, #3725, .T. ) ;
#18303 = DIRECTION ( 'NONE',  ( -0.000000000000000000, 1.000000000000000000, -0.000000000000000000 ) ) ;
#18304 = DIRECTION ( 'NONE',  ( 0.000000000000000000, -0.5000000000000009992, -0.8660254037844380415 ) ) ;
#18305 = VERTEX_POINT ( 'NONE', #9779 ) ;
#18306 = CIRCLE ( 'NONE', #20611, 2.055000000000001492 ) ;
#18307 = VECTOR ( 'NONE', #15371, 1000.000000000000000 ) ;
#18308 = DIRECTION ( 'NONE',  ( 0.5000000000000013323, -0.8660254037844379305, 0.000000000000000000 ) ) ;
#18309 = DIRECTION ( 'NONE',  ( 0.000000000000000000, 0.000000000000000000, 1.000000000000000000 ) ) ;
#18310 = ORIENTED_EDGE ( 'NONE', *, *, #15211, .F. ) ;
#18311 = CARTESIAN_POINT ( 'NONE',  ( 281.2440776823444253, 268.3679143846943020, 147.1132285165672329 ) ) ;
#18312 = CARTESIAN_POINT ( 'NONE',  ( 2.100000000000000089, 0.000000000000000000, -0.2800830152838844622 ) ) ;
#18313 = VERTEX_POINT ( 'NONE', #13570 ) ;
#18314 = EDGE_CURVE ( 'NONE', #10087, #18017, #12970, .T. ) ;
#18315 = AXIS2_PLACEMENT_3D ( 'NONE', #8072, #466, #11469 ) ;
#18316 = CYLINDRICAL_SURFACE ( 'NONE', #14488, 2.500000000000002220 ) ;
#18317 = CARTESIAN_POINT ( 'NONE',  ( -31.74999999999994316, 0.000000000000000000, 0.000000000000000000 ) ) ;
#18318 =( REPRESENTATION_RELATIONSHIP ('NONE','NONE', #10127, #18083 ) REPRESENTATION_RELATIONSHIP_WITH_TRANSFORMATION ( #7904 )SHAPE_REPRESENTATION_RELATIONSHIP( ) );
#18319 = DIRECTION ( 'NONE',  ( 1.000000000000000000, 0.000000000000000000, 0.000000000000000000 ) ) ;
#18320 = ORIENTED_EDGE ( 'NONE', *, *, #3849, .F. ) ;
#18321 = DIRECTION ( 'NONE',  ( 1.000000000000000000, 0.000000000000000000, -0.000000000000000000 ) ) ;
#18322 = CARTESIAN_POINT ( 'NONE',  ( -281.4928932188135491, -129.2000000000000455, 152.4000000000014268 ) ) ;
#18323 = ADVANCED_FACE ( 'NONE', ( #5797 ), #13676, .F. ) ;
#18324 = FACE_OUTER_BOUND ( 'NONE', #5206, .T. ) ;
#18325 = ORIENTED_EDGE ( 'NONE', *, *, #19088, .T. ) ;
#18326 = ORIENTED_EDGE ( 'NONE', *, *, #11955, .T. ) ;
#18327 = CARTESIAN_POINT ( 'NONE',  ( 7.894787914004607998, 1.243647571710251278E-13, -7.591390474663425536 ) ) ;
#18328 = APPLICATION_PROTOCOL_DEFINITION ( 'draft international standard', 'automotive_design', 1998, #19547 ) ;
#18329 = FACE_OUTER_BOUND ( 'NONE', #11912, .T. ) ;
#18330 = ADVANCED_FACE ( 'NONE', ( #2512 ), #3952, .T. ) ;
#18331 = EDGE_CURVE ( 'NONE', #12484, #1796, #958, .T. ) ;
#18332 = DIRECTION ( 'NONE',  ( -1.000000000000000000, -0.000000000000000000, -0.000000000000000000 ) ) ;
#18333 = LINE ( 'NONE', #16884, #8988 ) ;
#18334 = ORIENTED_EDGE ( 'NONE', *, *, #18454, .F. ) ;
#18335 = CARTESIAN_POINT ( 'NONE',  ( -16.52066876451827326, -18.83467029480909005, 145.0000119999999697 ) ) ;
#18336 = CONICAL_SURFACE ( 'NONE', #14893, 4.171999999999999709, 0.7853981633974613796 ) ;
#18337 = CIRCLE ( 'NONE', #23360, 5.200000000000028599 ) ;
#18338 = UNCERTAINTY_MEASURE_WITH_UNIT (LENGTH_MEASURE( 1.000000000000000082E-05 ), #959, 'distance_accuracy_value', 'NONE');
#18339 = AXIS2_PLACEMENT_3D ( 'NONE', #8272, #11567, #17212 ) ;
#18340 = PLANE ( 'NONE',  #13708 ) ;
#18341 = CYLINDRICAL_SURFACE ( 'NONE', #15704, 7.500000000000007105 ) ;
#18342 = VERTEX_POINT ( 'NONE', #17028 ) ;
#18343 = FACE_OUTER_BOUND ( 'NONE', #6425, .T. ) ;
#18344 = EDGE_LOOP ( 'NONE', ( #13803, #4965, #17724, #15007 ) ) ;
#18345 = EDGE_CURVE ( 'NONE', #20673, #2323, #22297, .T. ) ;
#18346 = VECTOR ( 'NONE', #2205, 1000.000000000000000 ) ;
#18347 = DIRECTION ( 'NONE',  ( -0.000000000000000000, -0.000000000000000000, 1.000000000000000000 ) ) ;
#18348 = EDGE_LOOP ( 'NONE', ( #14383, #12222, #10753, #4198 ) ) ;
#18349 = DIRECTION ( 'NONE',  ( -1.000000000000000000, -0.000000000000000000, -0.000000000000000000 ) ) ;
#18350 = DIRECTION ( 'NONE',  ( 0.000000000000000000, 0.000000000000000000, 1.000000000000000000 ) ) ;
#18351 = EDGE_CURVE ( 'NONE', #1816, #1127, #2498, .T. ) ;
#18352 = SURFACE_STYLE_FILL_AREA ( #3505 ) ;
#18353 = CARTESIAN_POINT ( 'NONE',  ( 0.000000000000000000, 1.865214261513747767E-15, -145.0000119999999697 ) ) ;
#18354 = CARTESIAN_POINT ( 'NONE',  ( 20.00000000000000000, -1000.000000000000000, -138.9999999999999716 ) ) ;
#18355 = ADVANCED_FACE ( 'NONE', ( #13411 ), #2129, .F. ) ;
#18356 = DIRECTION ( 'NONE',  ( 1.000000000000000000, 0.000000000000000000, -0.000000000000000000 ) ) ;
#18357 = ORIENTED_EDGE ( 'NONE', *, *, #7055, .T. ) ;
#18358 = DIRECTION ( 'NONE',  ( -0.000000000000000000, -0.000000000000000000, -1.000000000000000000 ) ) ;
#18359 = DIRECTION ( 'NONE',  ( 0.000000000000000000, 0.000000000000000000, 1.000000000000000000 ) ) ;
#18361 = ORIENTED_EDGE ( 'NONE', *, *, #14952, .T. ) ;
#18360 = ORIENTED_EDGE ( 'NONE', *, *, #5004, .F. ) ;
#18362 = CARTESIAN_POINT ( 'NONE',  ( -293.2000000000010118, -29.99999999999912959, -105.0000000000002416 ) ) ;
#18363 = CYLINDRICAL_SURFACE ( 'NONE', #18881, 2.500000000000002220 ) ;
#18364 = CIRCLE ( 'NONE', #22221, 5.249999999999949374 ) ;
#18365 = CARTESIAN_POINT ( 'NONE',  ( 280.9952621458755857, 268.8927021017107108, -146.8958543268121559 ) ) ;
#18366 = ORIENTED_EDGE ( 'NONE', *, *, #21968, .T. ) ;
#18367 = DIRECTION ( 'NONE',  ( 0.000000000000000000, 0.000000000000000000, 1.000000000000000000 ) ) ;
#18368 = CARTESIAN_POINT ( 'NONE',  ( -69.99999999999997158, -112.6666666666667140, 148.0000000000000000 ) ) ;
#18369 = ORIENTED_EDGE ( 'NONE', *, *, #18746, .F. ) ;
#18370 = DIRECTION ( 'NONE',  ( 1.000000000000000000, 0.000000000000000000, 0.000000000000000000 ) ) ;
#18371 = DIRECTION ( 'NONE',  ( 0.6964005597823107463, -0.7176533009294141507, 6.982962677686266711E-15 ) ) ;
#18372 = AXIS2_PLACEMENT_3D ( 'NONE', #20646, #18829, #503 ) ;
#18373 = CONTEXT_DEPENDENT_SHAPE_REPRESENTATION ( #3684, #15671 ) ;
#18374 = EDGE_LOOP ( 'NONE', ( #12645, #14216 ) ) ;
#18375 = CARTESIAN_POINT ( 'NONE',  ( 125.2206635291107943, -1091.349901830162025, 27.82811892742366311 ) ) ;
#18376 = EDGE_LOOP ( 'NONE', ( #23218, #4072, #1466, #5632 ) ) ;
#18377 = AXIS2_PLACEMENT_3D ( 'NONE', #12960, #7367, #22198 ) ;
#18378 = DIRECTION ( 'NONE',  ( -0.5000000000000034417, 0.000000000000000000, 0.8660254037844367092 ) ) ;
#18379 = CARTESIAN_POINT ( 'NONE',  ( 134.0852850658430384, 77.75691219176937352, 30.65186413114637531 ) ) ;
#18380 = ADVANCED_FACE ( 'NONE', ( #689 ), #4190, .F. ) ;
#18381 = CARTESIAN_POINT ( 'NONE',  ( 3.999999999999998224, 2.472263674411418588, -3.687027874309861897 ) ) ;
#18382 = LINE ( 'NONE', #5951, #4003 ) ;
#18383 = DIRECTION ( 'NONE',  ( 1.000000000000000000, 0.000000000000000000, 0.000000000000000000 ) ) ;
#18384 = DIRECTION ( 'NONE',  ( 0.000000000000000000, 0.000000000000000000, -1.000000000000000000 ) ) ;
#18385 = VERTEX_POINT ( 'NONE', #13551 ) ;
#18386 = CARTESIAN_POINT ( 'NONE',  ( 0.000000000000000000, 0.000000000000000000, 0.000000000000000000 ) ) ;
#18387 = PLANE ( 'NONE',  #8019 ) ;
#18388 = CARTESIAN_POINT ( 'NONE',  ( 7.897850199329715437, -1.533397866934079312, -7.634054012537967893 ) ) ;
#18389 = AXIS2_PLACEMENT_3D ( 'NONE', #18679, #9532, #13785 ) ;
#18390 = ORIENTED_EDGE ( 'NONE', *, *, #21277, .F. ) ;
#18391 = CARTESIAN_POINT ( 'NONE',  ( 280.8716261326570134, 269.1405375976307255, -146.7502846751312120 ) ) ;
#18392 = DIRECTION ( 'NONE',  ( -1.000000000000000000, 0.000000000000000000, 0.000000000000000000 ) ) ;
#18393 = AXIS2_PLACEMENT_3D ( 'NONE', #22109, #12638, #19948 ) ;
#18394 = AXIS2_PLACEMENT_3D ( 'NONE', #7610, #389, #9694 ) ;
#18395 = FACE_OUTER_BOUND ( 'NONE', #11875, .T. ) ;
#18396 = DIRECTION ( 'NONE',  ( -0.000000000000000000, -0.000000000000000000, 1.000000000000000000 ) ) ;
#18397 = CARTESIAN_POINT ( 'NONE',  ( 0.000000000000000000, 0.000000000000000000, 20.00000000000000000 ) ) ;
#18398 = ORIENTED_EDGE ( 'NONE', *, *, #10358, .T. ) ;
#18399 = LINE ( 'NONE', #18631, #12760 ) ;
#18400 = ORIENTED_EDGE ( 'NONE', *, *, #11514, .F. ) ;
#18401 = CARTESIAN_POINT ( 'NONE',  ( -100.0000000000000000, 249.9999999999999716, 125.0000000000000284 ) ) ;
#18402 = CARTESIAN_POINT ( 'NONE',  ( 0.000000000000000000, 0.000000000000000000, -0.5251556536572846712 ) ) ;
#18403 = ORIENTED_EDGE ( 'NONE', *, *, #6269, .F. ) ;
#18404 = CIRCLE ( 'NONE', #8803, 2.649999999999971934 ) ;
#18405 = DIRECTION ( 'NONE',  ( -0.000000000000000000, 1.000000000000000000, -3.469446951953613794E-15 ) ) ;
#18406 = CARTESIAN_POINT ( 'NONE',  ( 3.750000000000004441, -6.495190528383289141, 0.000000000000000000 ) ) ;
#18407 = EDGE_CURVE ( 'NONE', #5651, #5818, #16873, .T. ) ;
#18408 = CARTESIAN_POINT ( 'NONE',  ( -1.250000000000000444, -7.938566201357367902, -7.198902722707430257 ) ) ;
#18409 = DIRECTION ( 'NONE',  ( 1.000000000000000000, -0.000000000000000000, 6.982962677686266711E-15 ) ) ;
#18411 = AXIS2_PLACEMENT_3D ( 'NONE', #3887, #11296, #18603 ) ;
#18410 = LINE ( 'NONE', #5398, #4587 ) ;
#18412 = LINE ( 'NONE', #20582, #21572 ) ;
#18413 = FACE_BOUND ( 'NONE', #6635, .T. ) ;
#18414 = AXIS2_PLACEMENT_3D ( 'NONE', #9339, #20652, #18834 ) ;
#18415 = ORIENTED_EDGE ( 'NONE', *, *, #4893, .T. ) ;
#18416 = EDGE_LOOP ( 'NONE', ( #6809, #13875, #19720, #2579 ) ) ;
#18417 = CYLINDRICAL_SURFACE ( 'NONE', #15340, 25.00000000000000000 ) ;
#18418 = CARTESIAN_POINT ( 'NONE',  ( 2.500000000000002220, 1.178949249685218970, 2.041999999999998483 ) ) ;
#18419 = EDGE_CURVE ( 'NONE', #13534, #13337, #20370, .T. ) ;
#18420 = ORIENTED_EDGE ( 'NONE', *, *, #7429, .T. ) ;
#18421 = CARTESIAN_POINT ( 'NONE',  ( 8.354409714504226869, 5.621796044507131107, 200.0000120000000265 ) ) ;
#18422 = CARTESIAN_POINT ( 'NONE',  ( 1.015826369459276846, -8.073766409988136772, -7.642786413614194529 ) ) ;
#18423 = EDGE_LOOP ( 'NONE', ( #22975, #15292 ) ) ;
#18424 = CARTESIAN_POINT ( 'NONE',  ( 279.9999999999999432, 272.9999999999999432, 145.0000000000000284 ) ) ;
#18425 = DIRECTION ( 'NONE',  ( -1.000000000000000000, 0.000000000000000000, 0.000000000000000000 ) ) ;
#18426 = EDGE_CURVE ( 'NONE', #17715, #21835, #12606, .T. ) ;
#18427 = VERTEX_POINT ( 'NONE', #220 ) ;
#18428 = VECTOR ( 'NONE', #9434, 1000.000000000000000 ) ;
#18429 = AXIS2_PLACEMENT_3D ( 'NONE', #1626, #22031, #12903 ) ;
#18430 = CARTESIAN_POINT ( 'NONE',  ( -45.00000000000000000, 250.0000000000000000, 0.000000000000000000 ) ) ;
#18431 = DIRECTION ( 'NONE',  ( 0.000000000000000000, 0.000000000000000000, -1.000000000000000000 ) ) ;
#18432 = VECTOR ( 'NONE', #22430, 1000.000000000000000 ) ;
#18433 = CIRCLE ( 'NONE', #1084, 2.500000000000000888 ) ;
#18434 = CARTESIAN_POINT ( 'NONE',  ( -5.036189803708989388, -8.737863883542578591, 200.0000120000000265 ) ) ;
#18435 = ORIENTED_EDGE ( 'NONE', *, *, #6533, .F. ) ;
#18436 = DIRECTION ( 'NONE',  ( -0.000000000000000000, -0.000000000000000000, 1.000000000000000000 ) ) ;
#18437 = CARTESIAN_POINT ( 'NONE',  ( -136.3944205523261815, -1073.631384736298514, 32.17229779615536955 ) ) ;
#18438 = FILL_AREA_STYLE ('',( #16760 ) ) ;
#18439 = ORIENTED_EDGE ( 'NONE', *, *, #17266, .F. ) ;
#18440 = ORIENTED_EDGE ( 'NONE', *, *, #4149, .T. ) ;
#18441 = CARTESIAN_POINT ( 'NONE',  ( 7.897836333153806621, 1.530409084195003988, -7.633857274177628049 ) ) ;
#18442 = APPLICATION_PROTOCOL_DEFINITION ( 'draft international standard', 'automotive_design', 1998, #23255 ) ;
#18443 = CARTESIAN_POINT ( 'NONE',  ( 4.000000000000000000, 2.309401076758497151, -3.433295621305379353 ) ) ;
#18444 = LINE ( 'NONE', #22308, #3776 ) ;
#18445 = CARTESIAN_POINT ( 'NONE',  ( 4.000000000000000000, 0.000000000000000000, 0.000000000000000000 ) ) ;
#18446 = TOROIDAL_SURFACE ( 'NONE', #12717, 6.500000000000000888, 1.500000000000000000 ) ;
#18447 = EDGE_LOOP ( 'NONE', ( #16867, #6220, #19319, #6032 ) ) ;
#18448 = AXIS2_PLACEMENT_3D ( 'NONE', #15806, #4349, #14012 ) ;
#18449 = DIRECTION ( 'NONE',  ( -1.000000000000000000, 2.220299922379604070E-16, 0.000000000000000000 ) ) ;
#18450 = AXIS2_PLACEMENT_3D ( 'NONE', #3053, #12281, #19352 ) ;
#18451 = ADVANCED_FACE ( 'NONE', ( #578 ), #6004, .F. ) ;
#18452 = VECTOR ( 'NONE', #23804, 1000.000000000000000 ) ;
#18453 = CIRCLE ( 'NONE', #8825, 4.000000000000000000 ) ;
#18454 = EDGE_CURVE ( 'NONE', #19875, #3015, #5228, .T. ) ;
#18455 = EDGE_CURVE ( 'NONE', #5006, #539, #18662, .T. ) ;
#18456 = PRODUCT_DEFINITION_CONTEXT ( 'detailed design', #7365, 'design' ) ;
#18457 = CIRCLE ( 'NONE', #7679, 2.500000000000000444 ) ;
#18458 = APPLICATION_CONTEXT ( 'automotive_design' ) ;
#18459 = DIRECTION ( 'NONE',  ( 1.000000000000000000, 0.000000000000000000, 0.000000000000000000 ) ) ;
#18460 = EDGE_CURVE ( 'NONE', #14699, #17768, #10068, .T. ) ;
#18461 = LINE ( 'NONE', #2276, #11491 ) ;
#18462 = EDGE_CURVE ( 'NONE', #21409, #21406, #3651, .T. ) ;
#18463 = EDGE_LOOP ( 'NONE', ( #17151, #20087, #16695, #12912 ) ) ;
#18465 = EDGE_CURVE ( 'NONE', #5557, #1663, #21578, .T. ) ;
#18464 = DIRECTION ( 'NONE',  ( 0.000000000000000000, 1.000000000000000000, -1.224646799147353207E-16 ) ) ;
#18466 = VERTEX_POINT ( 'NONE', #12451 ) ;
#18467 = AXIS2_PLACEMENT_3D ( 'NONE', #8039, #20701, #20467 ) ;
#18468 = AXIS2_PLACEMENT_3D ( 'NONE', #8890, #16254, #20092 ) ;
#18470 = CARTESIAN_POINT ( 'NONE',  ( -79.99999999999995737, -138.0000000000000284, 0.000000000000000000 ) ) ;
#18469 = CIRCLE ( 'NONE', #6917, 2.055000000000001492 ) ;
#18471 = CIRCLE ( 'NONE', #11193, 2.649999999999971934 ) ;
#18473 = AXIS2_PLACEMENT_3D ( 'NONE', #6435, #19457, #8113 ) ;
#18472 = CARTESIAN_POINT ( 'NONE',  ( -285.2000000000011255, -29.99999999999898037, -107.6499999999999631 ) ) ;
#18474 = ORIENTED_EDGE ( 'NONE', *, *, #20932, .F. ) ;
#18475 = CARTESIAN_POINT ( 'NONE',  ( -128.7717867965307903, 86.27213916325827370, -27.99555145635496700 ) ) ;
#18476=STYLED_ITEM('',(#23927),#3850);
#18477 = AXIS2_PLACEMENT_3D ( 'NONE', #22655, #13549, #1029 ) ;
#18478 = LINE ( 'NONE', #14874, #12388 ) ;
#18479 = CARTESIAN_POINT ( 'NONE',  ( -11.07878015919983916, -1022.470824010819570, 145.0000119999999697 ) ) ;
#18480 = CARTESIAN_POINT ( 'NONE',  ( -282.2000000000000455, 268.0905802150184627, -146.3673618604586579 ) ) ;
#18481 = DIRECTION ( 'NONE',  ( 0.000000000000000000, 0.000000000000000000, 1.000000000000000000 ) ) ;
#18482 = DIRECTION ( 'NONE',  ( -0.000000000000000000, 1.000000000000000000, 0.000000000000000000 ) ) ;
#18483 = ORIENTED_EDGE ( 'NONE', *, *, #9820, .T. ) ;
#18484 = DIRECTION ( 'NONE',  ( -0.000000000000000000, 1.000000000000000000, 1.224646799147353207E-16 ) ) ;
#18485 = CARTESIAN_POINT ( 'NONE',  ( -44.80746418436648071, -137.9031948627975908, -90.00000000000000000 ) ) ;
#18486 =( LENGTH_UNIT ( ) NAMED_UNIT ( * ) SI_UNIT ( .MILLI., .METRE. ) );
#18488 = ORIENTED_EDGE ( 'NONE', *, *, #9417, .F. ) ;
#18487 = ORIENTED_EDGE ( 'NONE', *, *, #6202, .F. ) ;
#18489 = DIRECTION ( 'NONE',  ( 6.123233995736766036E-17, -1.000000000000000000, 0.000000000000000000 ) ) ;
#18491 = CIRCLE ( 'NONE', #1539, 20.00000000000000000 ) ;
#18490 = AXIS2_PLACEMENT_3D ( 'NONE', #11311, #18621, #9475 ) ;
#18492 = CARTESIAN_POINT ( 'NONE',  ( -136.1034519145107993, -1074.167893320492567, -27.57920702976961280 ) ) ;
#18493 = CARTESIAN_POINT ( 'NONE',  ( 280.8708543776411943, 269.1520027839448517, -146.7592670532759485 ) ) ;
#18494 = AXIS2_PLACEMENT_3D ( 'NONE', #20815, #15045, #20925 ) ;
#18495 = VECTOR ( 'NONE', #3609, 1000.000000000000000 ) ;
#18496 = ORIENTED_EDGE ( 'NONE', *, *, #2348, .T. ) ;
#18497 = CARTESIAN_POINT ( 'NONE',  ( -2.999999999999995559, 0.000000000000000000, 0.000000000000000000 ) ) ;
#18498 = EDGE_CURVE ( 'NONE', #1617, #15162, #19384, .T. ) ;
#18499 = EDGE_LOOP ( 'NONE', ( #7569, #8108, #22671, #16966 ) ) ;
#18500 = ADVANCED_FACE ( 'NONE', ( #6723 ), #21449, .T. ) ;
#18501 = DIRECTION ( 'NONE',  ( 0.000000000000000000, 0.000000000000000000, 1.000000000000000000 ) ) ;
#18502 = ORIENTED_EDGE ( 'NONE', *, *, #1346, .F. ) ;
#18503 = LINE ( 'NONE', #17060, #17336 ) ;
#18504 = CARTESIAN_POINT ( 'NONE',  ( 0.000000000000000000, 0.000000000000000000, 22.50000000000000000 ) ) ;
#18505 = ORIENTED_EDGE ( 'NONE', *, *, #23212, .T. ) ;
#18506 = CARTESIAN_POINT ( 'NONE',  ( -64.99999999999997158, -52.79999999999974847, 35.00000000000017764 ) ) ;
#18507 = AXIS2_PLACEMENT_3D ( 'NONE', #7142, #20415, #42 ) ;
#18508 = EDGE_LOOP ( 'NONE', ( #17047, #79 ) ) ;
#18509 =( REPRESENTATION_RELATIONSHIP ('NONE','NONE', #10127, #5587 ) REPRESENTATION_RELATIONSHIP_WITH_TRANSFORMATION ( #17915 )SHAPE_REPRESENTATION_RELATIONSHIP( ) );
#18510 = CARTESIAN_POINT ( 'NONE',  ( -129.2447185937761844, 85.56171376302357601, 30.81384172145500955 ) ) ;
#18511 = CARTESIAN_POINT ( 'NONE',  ( 6.250000000000000888, 5.051814855409225480, -7.198902722707425816 ) ) ;
#18512 = AXIS2_PLACEMENT_3D ( 'NONE', #11008, #12489, #20255 ) ;
#18513 = AXIS2_PLACEMENT_3D ( 'NONE', #4014, #13255, #22131 ) ;
#18514 = CARTESIAN_POINT ( 'NONE',  ( 0.3461262719736147297, -4.658553426539303821, -3.671615880910379381 ) ) ;
#18515 = CARTESIAN_POINT ( 'NONE',  ( -45.24999999999994316, 100.0000000000000000, -150.2000000000005571 ) ) ;
#18516 = CARTESIAN_POINT ( 'NONE',  ( 126.3653543294818178, 77.28387428943173632, -32.05499999999356930 ) ) ;
#18517 = VERTEX_POINT ( 'NONE', #16029 ) ;
#18518 =( LENGTH_UNIT ( ) NAMED_UNIT ( * ) SI_UNIT ( .MILLI., .METRE. ) );
#18519 = CARTESIAN_POINT ( 'NONE',  ( -7.499999999999999112, 41.99999999999998579, 100.0000000000000000 ) ) ;
#18520 = CARTESIAN_POINT ( 'NONE',  ( -20.63749999999999929, 0.000000000000000000, 0.000000000000000000 ) ) ;
#18521 = ORIENTED_EDGE ( 'NONE', *, *, #15339, .T. ) ;
#18522 = DIRECTION ( 'NONE',  ( 0.000000000000000000, -2.618450529776313049E-15, -1.000000000000000000 ) ) ;
#18523 = CARTESIAN_POINT ( 'NONE',  ( -44.99999999999997868, -59.79999999999936477, 195.0000000000001990 ) ) ;
#18524 = ORIENTED_EDGE ( 'NONE', *, *, #4695, .T. ) ;
#18525 = CARTESIAN_POINT ( 'NONE',  ( -282.2000000000014666, -127.0000000000000568, -144.9999999999999716 ) ) ;
#18526 = CARTESIAN_POINT ( 'NONE',  ( -281.4928932188134354, 267.8000000000000114, -147.1999999999999318 ) ) ;
#18527 = CARTESIAN_POINT ( 'NONE',  ( -35.00000000000000711, 4.286263797015349166E-15, -150.2000000000008981 ) ) ;
#18528 = CONTEXT_DEPENDENT_SHAPE_REPRESENTATION ( #9707, #8731 ) ;
#18529 = ORIENTED_EDGE ( 'NONE', *, *, #1586, .T. ) ;
#18530 = CARTESIAN_POINT ( 'NONE',  ( 158.0000000000000284, -500.0000000000000000, -32.64999999999995595 ) ) ;
#18531 = ORIENTED_EDGE ( 'NONE', *, *, #15374, .T. ) ;
#18532 = CARTESIAN_POINT ( 'NONE',  ( 145.9999999999998010, -209.9999999999996874, 30.00000000000641620 ) ) ;
#18533 =( LENGTH_UNIT ( ) NAMED_UNIT ( * ) SI_UNIT ( .MILLI., .METRE. ) );
#18534 = CARTESIAN_POINT ( 'NONE',  ( 2.500000000000000000, 2.629050547790028946E-15, 2.042000000000000259 ) ) ;
#18535 = ORIENTED_EDGE ( 'NONE', *, *, #925, .T. ) ;
#18536 = FILL_AREA_STYLE ('',( #19989 ) ) ;
#18537 = CARTESIAN_POINT ( 'NONE',  ( 122.9560050114703387, -1094.375960373424505, -29.67081494451410961 ) ) ;
#18538 = DIRECTION ( 'NONE',  ( 0.000000000000000000, 0.000000000000000000, 1.000000000000000000 ) ) ;
#18539 = DIRECTION ( 'NONE',  ( -1.000000000000000000, 1.408839003528726857E-14, 6.982962677686266711E-15 ) ) ;
#18540 = CARTESIAN_POINT ( 'NONE',  ( -7.500000000000000000, 4.330127018922191873, -7.422398894150032511 ) ) ;
#18541 = DIRECTION ( 'NONE',  ( 0.000000000000000000, 0.000000000000000000, 1.000000000000000000 ) ) ;
#18542 = DIRECTION ( 'NONE',  ( 1.000000000000000000, 0.000000000000000000, 0.000000000000000000 ) ) ;
#18543 = ORIENTED_EDGE ( 'NONE', *, *, #3452, .F. ) ;
#18544 = FACE_OUTER_BOUND ( 'NONE', #20596, .T. ) ;
#18545 = CARTESIAN_POINT ( 'NONE',  ( 281.4928932188133786, -132.2000000000000455, 7.703011046602857601E-15 ) ) ;
#18546 = VERTEX_POINT ( 'NONE', #5045 ) ;
#18547 = EDGE_CURVE ( 'NONE', #21466, #640, #1359, .T. ) ;
#18548 = CARTESIAN_POINT ( 'NONE',  ( -6.259644161404860030E-16, -4.618802153517027165, -5.000000000000000000 ) ) ;
#18549 = CARTESIAN_POINT ( 'NONE',  ( 1.500000000000001332, 0.000000000000000000, 0.000000000000000000 ) ) ;
#18550 = DIRECTION ( 'NONE',  ( 0.000000000000000000, 0.000000000000000000, -1.000000000000000000 ) ) ;
#18551 = EDGE_CURVE ( 'NONE', #15868, #9794, #8414, .T. ) ;
#18552 = ORIENTED_EDGE ( 'NONE', *, *, #14777, .T. ) ;
#18553 = DIRECTION ( 'NONE',  ( 1.000000000000000000, 0.000000000000000000, -0.000000000000000000 ) ) ;
#18554 = CARTESIAN_POINT ( 'NONE',  ( -4.000000000000000000, 0.9868501483902560878, -0.09357334158579519445 ) ) ;
#18555 = EDGE_CURVE ( 'NONE', #21242, #12669, #16808, .T. ) ;
#18556 = CARTESIAN_POINT ( 'NONE',  ( 9.999999999999998224, 6.123233995736764310E-16, 200.0000060000000133 ) ) ;
#18557 = ORIENTED_EDGE ( 'NONE', *, *, #4795, .F. ) ;
#18558 = CARTESIAN_POINT ( 'NONE',  ( -282.2000000000008981, 30.00000000000101963, -105.0000000000000142 ) ) ;
#18559 = CARTESIAN_POINT ( 'NONE',  ( 155.0000000000000284, -500.0000000000000000, 30.00000000000001421 ) ) ;
#18560 = ADVANCED_FACE ( 'NONE', ( #15914 ), #8195, .F. ) ;
#18561 = PRESENTATION_STYLE_ASSIGNMENT (( #20729 ) ) ;
#18562 = EDGE_LOOP ( 'NONE', ( #18008, #9191, #18310 ) ) ;
#18563 = DIRECTION ( 'NONE',  ( 0.000000000000000000, -1.000000000000000000, -5.286776307738891306E-15 ) ) ;
#18564 = SHAPE_DEFINITION_REPRESENTATION ( #16548, #4684 ) ;
#18565 = PLANE ( 'NONE',  #7735 ) ;
#18566 = CARTESIAN_POINT ( 'NONE',  ( 158.0000000000000568, -557.0000000000000000, 56.99999999999998579 ) ) ;
#18567 = DIRECTION ( 'NONE',  ( 0.000000000000000000, -2.618450529776326854E-15, -1.000000000000000000 ) ) ;
#18568 = ORIENTED_EDGE ( 'NONE', *, *, #15244, .F. ) ;
#18569 = ORIENTED_EDGE ( 'NONE', *, *, #12166, .F. ) ;
#18570 = DIRECTION ( 'NONE',  ( -0.000000000000000000, -0.000000000000000000, 1.000000000000000000 ) ) ;
#18571 = ORIENTED_EDGE ( 'NONE', *, *, #8816, .T. ) ;
#18572 = DIRECTION ( 'NONE',  ( -1.000000000000000000, -0.000000000000000000, -0.000000000000000000 ) ) ;
#18573 = DIRECTION ( 'NONE',  ( 1.000000000000000000, -1.408839003528726857E-14, -6.982962677686266711E-15 ) ) ;
#18574 = ORIENTED_EDGE ( 'NONE', *, *, #1443, .F. ) ;
#18575 = FACE_OUTER_BOUND ( 'NONE', #7273, .T. ) ;
#18576 = CIRCLE ( 'NONE', #11306, 2.041999999999999815 ) ;
#18577 = EDGE_CURVE ( 'NONE', #22067, #3718, #6401, .T. ) ;
#18578 = ORIENTED_EDGE ( 'NONE', *, *, #7960, .T. ) ;
#18579 = DIRECTION ( 'NONE',  ( 6.640089860198304064E-16, 1.000000000000000000, -3.495664435217746987E-15 ) ) ;
#18580 = ADVANCED_FACE ( 'NONE', ( #8657 ), #15797, .F. ) ;
#18581 = PLANE ( 'NONE',  #531 ) ;
#18582 = VERTEX_POINT ( 'NONE', #4549 ) ;
#18583 = CARTESIAN_POINT ( 'NONE',  ( -127.9021285790837510, 87.55595642181940264, -27.49999999999351985 ) ) ;
#18584 = ADVANCED_FACE ( 'NONE', ( #14236 ), #23377, .F. ) ;
#18585 = DIRECTION ( 'NONE',  ( -1.000000000000000000, 0.000000000000000000, 0.000000000000000000 ) ) ;
#18586 =( LENGTH_UNIT ( ) NAMED_UNIT ( * ) SI_UNIT ( .MILLI., .METRE. ) );
#18587 = CARTESIAN_POINT ( 'NONE',  ( 67.35000000000002274, -87.33333333333332860, 148.0000000000000000 ) ) ;
#18588 = CARTESIAN_POINT ( 'NONE',  ( 125.9649699199272277, -1090.320686186013972, -29.83126738556716262 ) ) ;
#18589 = EDGE_CURVE ( 'NONE', #13209, #22845, #21425, .T. ) ;
#18590 = CARTESIAN_POINT ( 'NONE',  ( -130.4031948627974486, 44.80746418436699940, 90.00000000000000000 ) ) ;
#18591 = ORIENTED_EDGE ( 'NONE', *, *, #6502, .T. ) ;
#18592 = DIRECTION ( 'NONE',  ( 0.000000000000000000, 0.000000000000000000, 1.000000000000000000 ) ) ;
#18593 = CARTESIAN_POINT ( 'NONE',  ( -4.250000000000000000, 5.204748896376250699E-16, -9.449444346342714240 ) ) ;
#18594 = VECTOR ( 'NONE', #23049, 1000.000000000000000 ) ;
#18596 = ORIENTED_EDGE ( 'NONE', *, *, #11816, .F. ) ;
#18595 = VERTEX_POINT ( 'NONE', #11970 ) ;
#18597 = CARTESIAN_POINT ( 'NONE',  ( 45.00000000000002132, 240.0000000000000000, 0.000000000000000000 ) ) ;
#18598 = CARTESIAN_POINT ( 'NONE',  ( 158.0000000000000284, -490.0000000000000000, 9.066821367772113093E-13 ) ) ;
#18599 = DIRECTION ( 'NONE',  ( -1.000000000000000000, 0.000000000000000000, 0.000000000000000000 ) ) ;
#18600 = VERTEX_POINT ( 'NONE', #19278 ) ;
#18601 = CARTESIAN_POINT ( 'NONE',  ( -134.7157571289267821, -1076.659463591458461, 28.74299381080683347 ) ) ;
#18602 = ORIENTED_EDGE ( 'NONE', *, *, #4860, .F. ) ;
#18603 = DIRECTION ( 'NONE',  ( 0.000000000000000000, 0.000000000000000000, -1.000000000000000000 ) ) ;
#18604 = VERTEX_POINT ( 'NONE', #10130 ) ;
#18605 = CARTESIAN_POINT ( 'NONE',  ( -145.0000000000000284, -5.062647941322544249E-13, -90.00000000000000000 ) ) ;
#18606 = VERTEX_POINT ( 'NONE', #4788 ) ;
#18607 = AXIS2_PLACEMENT_3D ( 'NONE', #2729, #4663, #17565 ) ;
#18608 = CARTESIAN_POINT ( 'NONE',  ( 124.4701338314438317, -1092.369831568442805, 32.50000000000646594 ) ) ;
#18609 = ORIENTED_EDGE ( 'NONE', *, *, #16433, .F. ) ;
#18610 = DIRECTION ( 'NONE',  ( 1.110223024625155594E-14, 0.000000000000000000, -1.000000000000000000 ) ) ;
#18611 = CARTESIAN_POINT ( 'NONE',  ( 1.411581201560190495E-15, 4.862606272033091592, -3.745885042887436622 ) ) ;
#18612 = DIRECTION ( 'NONE',  ( 0.000000000000000000, -0.000000000000000000, 1.000000000000000000 ) ) ;
#18613 = FACE_OUTER_BOUND ( 'NONE', #5136, .T. ) ;
#18614 = EDGE_CURVE ( 'NONE', #9739, #6820, #17476, .T. ) ;
#18615 = CARTESIAN_POINT ( 'NONE',  ( -282.1290760626067708, 268.3724317483737423, 146.2431816561009725 ) ) ;
#18616 = ADVANCED_FACE ( 'NONE', ( #2956 ), #15679, .F. ) ;
#18617 = CARTESIAN_POINT ( 'NONE',  ( 20.00000000000000000, -1000.000000000000000, 138.9999999999999716 ) ) ;
#18618 = AXIS2_PLACEMENT_3D ( 'NONE', #13263, #20570, #9607 ) ;
#18619 = VERTEX_POINT ( 'NONE', #12092 ) ;
#18620 = MECHANICAL_DESIGN_GEOMETRIC_PRESENTATION_REPRESENTATION (  '', ( #12137 ), #7447 ) ;
#18621 = DIRECTION ( 'NONE',  ( 0.000000000000000000, 0.000000000000000000, 1.000000000000000000 ) ) ;
#18622 = DIRECTION ( 'NONE',  ( 1.000000000000000000, 0.000000000000000000, 0.000000000000000000 ) ) ;
#18623 = CARTESIAN_POINT ( 'NONE',  ( 131.6943452429971728, 81.74110354019178715, -31.25700618919314522 ) ) ;
#18624 = CIRCLE ( 'NONE', #8242, 2.055000000000001492 ) ;
#18625 = DIRECTION ( 'NONE',  ( -0.000000000000000000, 0.000000000000000000, 1.000000000000000000 ) ) ;
#18626 = PLANE ( 'NONE',  #2151 ) ;
#18627 = CARTESIAN_POINT ( 'NONE',  ( -20.00000000000000000, -1000.000000000000000, -125.0000000000001137 ) ) ;
#18628 = DIRECTION ( 'NONE',  ( 0.000000000000000000, -0.8660254037844390407, -0.4999999999999993339 ) ) ;
#18629 = VERTEX_POINT ( 'NONE', #2845 ) ;
#18631 = CARTESIAN_POINT ( 'NONE',  ( 2.500000000000000000, 2.500728763858895382E-16, -2.041999999999999815 ) ) ;
#18630 = AXIS2_PLACEMENT_3D ( 'NONE', #17755, #8327, #1202 ) ;
#18632 = ORIENTED_EDGE ( 'NONE', *, *, #623, .F. ) ;
#18633 = DIRECTION ( 'NONE',  ( -6.486615240276975916E-15, -2.585650881802458380E-15, 1.000000000000000000 ) ) ;
#18634 = CARTESIAN_POINT ( 'NONE',  ( -67.34999999999996589, -112.6666666666667140, 124.9999999999999858 ) ) ;
#18635 = LINE ( 'NONE', #12911, #17145 ) ;
#18636 = ORIENTED_EDGE ( 'NONE', *, *, #13672, .T. ) ;
#18637 = DIRECTION ( 'NONE',  ( 0.000000000000000000, 0.000000000000000000, -1.000000000000000000 ) ) ;
#18638 = CARTESIAN_POINT ( 'NONE',  ( 123.8018707182395985, -1093.263712923000639, -27.75009929603930559 ) ) ;
#18639 = DIRECTION ( 'NONE',  ( 0.000000000000000000, 0.000000000000000000, 1.000000000000000000 ) ) ;
#18640 = DIRECTION ( 'NONE',  ( -1.000000000000000000, 0.000000000000000000, 0.000000000000000000 ) ) ;
#18641 = EDGE_CURVE ( 'NONE', #8313, #10712, #10243, .T. ) ;
#18642 = CARTESIAN_POINT ( 'NONE',  ( 0.000000000000000000, 0.000000000000000000, -90.00000000000000000 ) ) ;
#18643 = DIRECTION ( 'NONE',  ( 0.000000000000000000, -0.4999999999999993339, 0.8660254037844390407 ) ) ;
#18644 = CARTESIAN_POINT ( 'NONE',  ( 2.500000000000002220, 0.000000000000000000, 0.000000000000000000 ) ) ;
#18645 = EDGE_CURVE ( 'NONE', #13026, #14427, #10363, .T. ) ;
#18646 = EDGE_LOOP ( 'NONE', ( #6290, #22670, #6509, #8904 ) ) ;
#18647 = SURFACE_SIDE_STYLE ('',( #16314 ) ) ;
#18648 = DIRECTION ( 'NONE',  ( -0.000000000000000000, -0.000000000000000000, -1.000000000000000000 ) ) ;
#18649 = CARTESIAN_POINT ( 'NONE',  ( 158.0000000000000284, -500.0000000000000000, -29.99999999999997158 ) ) ;
#18650 = ORIENTED_EDGE ( 'NONE', *, *, #15211, .T. ) ;
#18651 = ORIENTED_EDGE ( 'NONE', *, *, #15203, .T. ) ;
#18652 = FACE_BOUND ( 'NONE', #14767, .T. ) ;
#18654 = CIRCLE ( 'NONE', #16370, 2.649999999999985700 ) ;
#18653 = CARTESIAN_POINT ( 'NONE',  ( -287.4000000000014552, -132.2000000000000455, 146.4928932188134638 ) ) ;
#18655 = AXIS2_PLACEMENT_3D ( 'NONE', #3368, #20266, #18459 ) ;
#18656 = CARTESIAN_POINT ( 'NONE',  ( 5.000000000000000000, 0.000000000000000000, 0.000000000000000000 ) ) ;
#18657 = ORIENTED_EDGE ( 'NONE', *, *, #6215, .F. ) ;
#18658 = CARTESIAN_POINT ( 'NONE',  ( -2.344047193898593395, -3.265465875126480455, -1.054683074273691752E-14 ) ) ;
#18659 = DIRECTION ( 'NONE',  ( 1.000000000000000000, 0.000000000000000000, 0.000000000000000000 ) ) ;
#18660 = FACE_OUTER_BOUND ( 'NONE', #22244, .T. ) ;
#18661 = ORIENTED_EDGE ( 'NONE', *, *, #12480, .T. ) ;
#18662 = LINE ( 'NONE', #19031, #14120 ) ;
#18663 = CARTESIAN_POINT ( 'NONE',  ( -64.99999999999997158, -56.79999999999975557, 35.00000000000019185 ) ) ;
#18664 = VECTOR ( 'NONE', #16839, 1000.000000000000000 ) ;
#18665 = CARTESIAN_POINT ( 'NONE',  ( -3.264650091097280831E-13, -4.796980096169642493, -3.721999068284424617 ) ) ;
#18666 = ORIENTED_EDGE ( 'NONE', *, *, #23579, .T. ) ;
#18667 = EDGE_CURVE ( 'NONE', #223, #13899, #18719, .T. ) ;
#18668 = CARTESIAN_POINT ( 'NONE',  ( -122.8605704798721803, 82.74225173005937961, -27.94499999999355921 ) ) ;
#18669 = APPLICATION_PROTOCOL_DEFINITION ( 'draft international standard', 'automotive_design', 1998, #3636 ) ;
#18670 = EDGE_CURVE ( 'NONE', #20231, #16162, #19214, .T. ) ;
#18671 = FACE_BOUND ( 'NONE', #8441, .T. ) ;
#18672 = VECTOR ( 'NONE', #8164, 1000.000000000000000 ) ;
#18673 = DIRECTION ( 'NONE',  ( 0.000000000000000000, 0.000000000000000000, -1.000000000000000000 ) ) ;
#18674 = FACE_OUTER_BOUND ( 'NONE', #19906, .T. ) ;
#18675 = VECTOR ( 'NONE', #21982, 1000.000000000000000 ) ;
#18676 = AXIS2_PLACEMENT_3D ( 'NONE', #14452, #10853, #9006 ) ;
#18677 = EDGE_LOOP ( 'NONE', ( #18072, #5552 ) ) ;
#18678 = ORIENTED_EDGE ( 'NONE', *, *, #1831, .T. ) ;
#18679 = CARTESIAN_POINT ( 'NONE',  ( 70.00000000000000000, -87.33333333333332860, 148.0000000000000000 ) ) ;
#18680 = CARTESIAN_POINT ( 'NONE',  ( 119.6158142514527327, -1087.367367941136308, 30.00000000000641620 ) ) ;
#18681 = PRODUCT_DEFINITION_CONTEXT ( 'detailed design', #20934, 'design' ) ;
#18682 = EDGE_CURVE ( 'NONE', #19800, #8431, #9494, .T. ) ;
#18683 = ORIENTED_EDGE ( 'NONE', *, *, #13767, .T. ) ;
#18684 = CARTESIAN_POINT ( 'NONE',  ( 145.0000000000000284, 0.000000000000000000, 90.00000000000000000 ) ) ;
#18685 = AXIS2_PLACEMENT_3D ( 'NONE', #21357, #19531, #6634 ) ;
#18686 = LINE ( 'NONE', #3853, #1425 ) ;
#18687 = ORIENTED_EDGE ( 'NONE', *, *, #7973, .T. ) ;
#18688 = CARTESIAN_POINT ( 'NONE',  ( 0.000000000000000000, 0.000000000000000000, 169.9999999999999716 ) ) ;
#18689 = AXIS2_PLACEMENT_3D ( 'NONE', #19535, #17860, #19412 ) ;
#18690 = CLOSED_SHELL ( 'NONE', ( #14259, #10820, #14773, #18204, #8052, #16530, #1618, #4931, #15909, #10778, #3701, #5362, #10361, #10019, #3628, #19804, #17737, #19060, #16965, #5921, #9328, #1557, #174, #7012, #11103, #6204, #3884 ) ) ;
#18691 = ORIENTED_EDGE ( 'NONE', *, *, #18849, .T. ) ;
#18692 = CARTESIAN_POINT ( 'NONE',  ( -2.700000000000001510, 0.000000000000000000, 0.000000000000000000 ) ) ;
#18693 = DIRECTION ( 'NONE',  ( 0.000000000000000000, -1.000000000000000000, 9.256405414277014607E-16 ) ) ;
#18694 = ORIENTED_EDGE ( 'NONE', *, *, #3737, .T. ) ;
#18695 = ORIENTED_EDGE ( 'NONE', *, *, #6799, .F. ) ;
#18696 = LINE ( 'NONE', #14994, #3837 ) ;
#18697 = CARTESIAN_POINT ( 'NONE',  ( -280.3118087683467365, 272.7329465209279533, -146.6795879751482801 ) ) ;
#18698 = AXIS2_PLACEMENT_3D ( 'NONE', #20977, #9653, #4435 ) ;
#18699 = CARTESIAN_POINT ( 'NONE',  ( 3.272451888078299564, -1024.838847803014232, 145.0000119999999697 ) ) ;
#18700 = DIRECTION ( 'NONE',  ( 0.000000000000000000, -1.000000000000000000, 0.000000000000000000 ) ) ;
#18701 = CYLINDRICAL_SURFACE ( 'NONE', #5768, 2.649999999999999467 ) ;
#18702 = DIRECTION ( 'NONE',  ( -1.000000000000000000, 0.000000000000000000, 0.000000000000000000 ) ) ;
#18703 = EDGE_CURVE ( 'NONE', #16256, #9824, #5146, .T. ) ;
#18704 = CARTESIAN_POINT ( 'NONE',  ( 4.000000000000000000, -2.309401076758516691, -0.4999999999999995559 ) ) ;
#18705 = ORIENTED_EDGE ( 'NONE', *, *, #17831, .F. ) ;
#18706 = EDGE_CURVE ( 'NONE', #20079, #16743, #11046, .T. ) ;
#18707 = FACE_BOUND ( 'NONE', #2047, .T. ) ;
#18708 = DIRECTION ( 'NONE',  ( -0.000000000000000000, 0.000000000000000000, 1.000000000000000000 ) ) ;
#18709 = ITEM_DEFINED_TRANSFORMATION ( 'NONE', 'NONE', #23520,  #11210 ) ;
#18711 = ORIENTED_EDGE ( 'NONE', *, *, #13329, .T. ) ;
#18710 = ORIENTED_EDGE ( 'NONE', *, *, #17021, .T. ) ;
#18712 = CYLINDRICAL_SURFACE ( 'NONE', #19269, 2.649999999999999467 ) ;
#18713 = DIRECTION ( 'NONE',  ( 1.350636282998972974E-14, 0.000000000000000000, -1.000000000000000000 ) ) ;
#18714 = EDGE_CURVE ( 'NONE', #1398, #14870, #611, .T. ) ;
#18715 = ORIENTED_EDGE ( 'NONE', *, *, #10977, .F. ) ;
#18716 = EDGE_CURVE ( 'NONE', #9513, #15265, #21799, .T. ) ;
#18717 = CARTESIAN_POINT ( 'NONE',  ( -134.8072682999800520, -1076.498424757946395, 28.47118012353581662 ) ) ;
#18718 = ORIENTED_EDGE ( 'NONE', *, *, #15938, .T. ) ;
#18719 = CIRCLE ( 'NONE', #16050, 145.0000000000000284 ) ;
#18720 = DIRECTION ( 'NONE',  ( -1.350636282998972974E-14, 0.000000000000000000, -1.000000000000000000 ) ) ;
#18721 = ORIENTED_EDGE ( 'NONE', *, *, #305, .F. ) ;
#18722 = DIRECTION ( 'NONE',  ( -0.000000000000000000, -0.000000000000000000, 1.000000000000000000 ) ) ;
#18723 = DIRECTION ( 'NONE',  ( 1.000000000000000000, 0.000000000000000000, 0.000000000000000000 ) ) ;
#18724 = ITEM_DEFINED_TRANSFORMATION ( 'NONE', 'NONE', #23152,  #11210 ) ;
#18725 = VERTEX_POINT ( 'NONE', #14360 ) ;
#18726 = PLANE ( 'NONE',  #10675 ) ;
#18727 = ORIENTED_EDGE ( 'NONE', *, *, #14501, .T. ) ;
#18728 = CARTESIAN_POINT ( 'NONE',  ( -280.6846668451111668, 271.7159870726003987, 148.4379565153279827 ) ) ;
#18729 = FILL_AREA_STYLE_COLOUR ( '', #11982 ) ;
#18730 = DIRECTION ( 'NONE',  ( -1.000000000000000000, 0.000000000000000000, 0.000000000000000000 ) ) ;
#18731 = DIRECTION ( 'NONE',  ( 0.000000000000000000, 0.000000000000000000, -1.000000000000000000 ) ) ;
#18732 = ORIENTED_EDGE ( 'NONE', *, *, #415, .F. ) ;
#18733 = CARTESIAN_POINT ( 'NONE',  ( -280.8708543776411943, 270.9956429438695409, -149.1582675804705218 ) ) ;
#18734 = AXIS2_PLACEMENT_3D ( 'NONE', #7531, #20930, #7780 ) ;
#18735 = VERTEX_POINT ( 'NONE', #18401 ) ;
#18736 = DIRECTION ( 'NONE',  ( 1.000000000000000000, 0.000000000000000000, 0.000000000000000000 ) ) ;
#18737 = ADVANCED_FACE ( 'NONE', ( #10966 ), #2142, .F. ) ;
#18738 = VECTOR ( 'NONE', #1736, 1000.000000000000000 ) ;
#18739 = DIRECTION ( 'NONE',  ( 0.000000000000000000, 0.000000000000000000, 1.000000000000000000 ) ) ;
#18740 = DIRECTION ( 'NONE',  ( -1.000000000000000000, 3.495664435217746592E-15, -0.000000000000000000 ) ) ;
#18741 = EDGE_CURVE ( 'NONE', #2917, #1785, #23724, .T. ) ;
#18742 = ADVANCED_FACE ( 'NONE', ( #21690 ), #18187, .T. ) ;
#18743 = CARTESIAN_POINT ( 'NONE',  ( 158.0000000000000284, -500.0000000000000000, 27.35000000000002629 ) ) ;
#18744 = CARTESIAN_POINT ( 'NONE',  ( -285.2300000000000182, 267.7999999999999545, -146.4928932188134354 ) ) ;
#18745 = EDGE_CURVE ( 'NONE', #21528, #9606, #13247, .T. ) ;
#18746 = EDGE_CURVE ( 'NONE', #13555, #3080, #9093, .T. ) ;
#18747 = AXIS2_PLACEMENT_3D ( 'NONE', #11019, #5441, #1328 ) ;
#18748 = CARTESIAN_POINT ( 'NONE',  ( 2.500000000000000000, 2.357898499370432166, -2.385244779468109755E-15 ) ) ;
#18749 = EDGE_CURVE ( 'NONE', #10685, #9425, #1525, .T. ) ;
#18750 = DIRECTION ( 'NONE',  ( 0.9289202219288174023, 0.3702799228849933955, 6.982962677686265922E-15 ) ) ;
#18751 = ITEM_DEFINED_TRANSFORMATION ( 'NONE', 'NONE', #8472,  #11210 ) ;
#18752 = ORIENTED_EDGE ( 'NONE', *, *, #4453, .T. ) ;
#18753 = CARTESIAN_POINT ( 'NONE',  ( -7.497491405671719455, 144.8060344827586334, 90.00000000000000000 ) ) ;
#18754 = VERTEX_POINT ( 'NONE', #14571 ) ;
#18755 = PLANE ( 'NONE',  #17364 ) ;
#18756 = DIRECTION ( 'NONE',  ( 1.000000000000000000, 0.000000000000000000, 0.000000000000000000 ) ) ;
#18757 = CARTESIAN_POINT ( 'NONE',  ( 52.00000000000000711, -135.7851947190609678, -3.814213562373143684 ) ) ;
#18758 = VERTEX_POINT ( 'NONE', #12807 ) ;
#18759 = CARTESIAN_POINT ( 'NONE',  ( -1.994931997373328159E-14, -8.660254037844390851, -1.000000000000000888 ) ) ;
#18760 = CARTESIAN_POINT ( 'NONE',  ( -31.74999999999995737, 0.000000000000000000, 0.000000000000000000 ) ) ;
#18761 = CARTESIAN_POINT ( 'NONE',  ( 2.500000000000000000, -2.629050547790028551E-15, -2.041999999999999815 ) ) ;
#18762 = FACE_BOUND ( 'NONE', #5695, .T. ) ;
#18763 = DIRECTION ( 'NONE',  ( -0.3090169943749517811, 0.9510565162951520879, 0.000000000000000000 ) ) ;
#18764 = CARTESIAN_POINT ( 'NONE',  ( -40.00000000000000000, 100.0000000000000000, 150.2000000000009550 ) ) ;
#18765 = AXIS2_PLACEMENT_3D ( 'NONE', #8765, #10593, #12977 ) ;
#18766 = DIRECTION ( 'NONE',  ( 1.000000000000000000, 0.000000000000000000, 0.000000000000000000 ) ) ;
#18767 =( REPRESENTATION_RELATIONSHIP ('NONE','NONE', #10127, #18083 ) REPRESENTATION_RELATIONSHIP_WITH_TRANSFORMATION ( #5732 )SHAPE_REPRESENTATION_RELATIONSHIP( ) );
#18768 = EDGE_LOOP ( 'NONE', ( #14929, #349, #21053, #7577 ) ) ;
#18769 = ADVANCED_FACE ( 'NONE', ( #8915 ), #18336, .T. ) ;
#18770 = CARTESIAN_POINT ( 'NONE',  ( -280.0000000000000568, 269.9999999999999432, 145.0000000000000284 ) ) ;
#18771 = VECTOR ( 'NONE', #14865, 1000.000000000000000 ) ;
#18772 = CARTESIAN_POINT ( 'NONE',  ( -129.6400180686271142, -1072.557589128678273, -29.99999999999356248 ) ) ;
#18773 = ORIENTED_EDGE ( 'NONE', *, *, #5930, .F. ) ;
#18774 = EDGE_LOOP ( 'NONE', ( #3021, #8777, #18773, #11675 ) ) ;
#18775 = CARTESIAN_POINT ( 'NONE',  ( 0.000000000000000000, 0.000000000000000000, 90.00000000000000000 ) ) ;
#18776 = CARTESIAN_POINT ( 'NONE',  ( 2.500000000000000000, 0.000000000000000000, 0.000000000000000000 ) ) ;
#18777 = DIRECTION ( 'NONE',  ( -0.000000000000000000, 1.000000000000000000, -3.495664435217746987E-15 ) ) ;
#18778 = ORIENTED_EDGE ( 'NONE', *, *, #17240, .F. ) ;
#18779 = EDGE_CURVE ( 'NONE', #9157, #15889, #22569, .T. ) ;
#18780 = CYLINDRICAL_SURFACE ( 'NONE', #16515, 25.00000000000000000 ) ;
#18781 = EDGE_CURVE ( 'NONE', #14870, #1398, #15280, .T. ) ;
#18782 = DIRECTION ( 'NONE',  ( 0.000000000000000000, 0.000000000000000000, -1.000000000000000000 ) ) ;
#18783 = TOROIDAL_SURFACE ( 'NONE', #2593, 2.700000000000000622, 0.2000000000000000111 ) ;
#18784 = DIRECTION ( 'NONE',  ( -2.775557561562891351E-17, 1.000000000000000000, 4.694093751100962712E-16 ) ) ;
#18785 = ORIENTED_EDGE ( 'NONE', *, *, #9323, .T. ) ;
#18786 = CARTESIAN_POINT ( 'NONE',  ( 281.1807969192696532, 269.4810649015076933, 149.9324007871373681 ) ) ;
#18787 = FACE_OUTER_BOUND ( 'NONE', #16127, .T. ) ;
#18788 = CIRCLE ( 'NONE', #9948, 2.649999999999999467 ) ;
#18789 = UNCERTAINTY_MEASURE_WITH_UNIT (LENGTH_MEASURE( 1.000000000000000082E-05 ), #15956, 'distance_accuracy_value', 'NONE');
#18790 =( NAMED_UNIT ( * ) PLANE_ANGLE_UNIT ( ) SI_UNIT ( $, .RADIAN. ) );
#18791 = ORIENTED_EDGE ( 'NONE', *, *, #8004, .F. ) ;
#18792 = DIRECTION ( 'NONE',  ( 1.110223024625155594E-14, 0.000000000000000000, -1.000000000000000000 ) ) ;
#18793 = CIRCLE ( 'NONE', #10741, 8.000000000000000000 ) ;
#18794 = PRODUCT_CONTEXT ( 'NONE', #22932, 'mechanical' ) ;
#18795 = FACE_OUTER_BOUND ( 'NONE', #8269, .T. ) ;
#18796 = DIRECTION ( 'NONE',  ( -0.000000000000000000, -0.000000000000000000, -1.000000000000000000 ) ) ;
#18797 = DIRECTION ( 'NONE',  ( 0.000000000000000000, 0.4999999999999980016, -0.8660254037844397068 ) ) ;
#18798 = ORIENTED_EDGE ( 'NONE', *, *, #3366, .T. ) ;
#18799 = ORIENTED_EDGE ( 'NONE', *, *, #17311, .F. ) ;
#18800 = CARTESIAN_POINT ( 'NONE',  ( 24.83884780301427853, -3.272451888078305782, 145.0000119999999697 ) ) ;
#18801 = FACE_OUTER_BOUND ( 'NONE', #8178, .T. ) ;
#18802 = AXIS2_PLACEMENT_3D ( 'NONE', #6952, #19970, #5601 ) ;
#18803 = AXIS2_PLACEMENT_3D ( 'NONE', #20210, #3660, #7306 ) ;
#18804 = CIRCLE ( 'NONE', #19194, 2.649999999999985700 ) ;
#18805 = ORIENTED_EDGE ( 'NONE', *, *, #2411, .F. ) ;
#18806 = CARTESIAN_POINT ( 'NONE',  ( -281.4928932188135491, 267.7999999999999545, 145.0000000000000284 ) ) ;
#18807 = CIRCLE ( 'NONE', #8423, 6.500000000000000888 ) ;
#18808 = DIRECTION ( 'NONE',  ( 1.000000000000000000, -0.000000000000000000, -0.000000000000000000 ) ) ;
#18809 = ORIENTED_EDGE ( 'NONE', *, *, #16733, .F. ) ;
#18810 = PLANE ( 'NONE',  #13371 ) ;
#18811 = ORIENTED_EDGE ( 'NONE', *, *, #15050, .F. ) ;
#18812 = PRESENTATION_STYLE_ASSIGNMENT (( #373 ) ) ;
#18813 = CARTESIAN_POINT ( 'NONE',  ( 1.118033988749894458, 2.877919977996280320E-15, -23.50000000000000000 ) ) ;
#18814 = ORIENTED_EDGE ( 'NONE', *, *, #14869, .T. ) ;
#18815 = ORIENTED_EDGE ( 'NONE', *, *, #21226, .T. ) ;
#18816 = LINE ( 'NONE', #494, #12384 ) ;
#18817 = AXIS2_PLACEMENT_3D ( 'NONE', #8787, #15683, #8306 ) ;
#18818 = CARTESIAN_POINT ( 'NONE',  ( 235.0000000000000284, -560.0000000000000000, 59.99999999999999289 ) ) ;
#18819 = AXIS2_PLACEMENT_3D ( 'NONE', #15071, #20955, #20581 ) ;
#18820 = DIRECTION ( 'NONE',  ( 0.000000000000000000, 0.000000000000000000, 1.000000000000000000 ) ) ;
#18821 = CIRCLE ( 'NONE', #2632, 5.249999999999973355 ) ;
#18822 = CARTESIAN_POINT ( 'NONE',  ( -280.7095819834008807, 269.8873946496624399, -145.3113419039144105 ) ) ;
#18823 = PLANE ( 'NONE',  #11989 ) ;
#18824 = DIRECTION ( 'NONE',  ( 0.000000000000000000, 0.000000000000000000, -1.000000000000000000 ) ) ;
#18825 = VECTOR ( 'NONE', #6552, 1000.000000000000000 ) ;
#18826 = LINE ( 'NONE', #2298, #4993 ) ;
#18827 = VERTEX_POINT ( 'NONE', #21910 ) ;
#18828 = CARTESIAN_POINT ( 'NONE',  ( -77.72886158240878274, 117.3074641843673049, 90.00000000000000000 ) ) ;
#18829 = DIRECTION ( 'NONE',  ( -1.000000000000000000, -0.000000000000000000, -0.000000000000000000 ) ) ;
#18830 = VECTOR ( 'NONE', #18188, 1000.000000000000000 ) ;
#18831 =( BOUNDED_SURFACE ( )  B_SPLINE_SURFACE ( 3, 2, ( 
 ( #7410, #5478, #8994 ),
 ( #2078, #14791, #9469 ),
 ( #20090, #3643, #1836 ),
 ( #3766, #23595, #13129 ),
 ( #11059, #22119, #1613 ),
 ( #23702, #18381, #9110 ) ),
 .UNSPECIFIED., .F., .F., .F. ) 
 B_SPLINE_SURFACE_WITH_KNOTS ( ( 4, 2, 4 ),
 ( 3, 3 ),
 ( 0.02027065861071770947, 0.02273072267836921331, 0.02519078674602071716 ),
 ( 0.000000000000000000, 1.000000000000000000 ),
 .UNSPECIFIED. ) 
 GEOMETRIC_REPRESENTATION_ITEM ( )  RATIONAL_B_SPLINE_SURFACE ( (
 ( 1.000000000000000000, 0.8047781708337304885, 1.000000000000000000),
 ( 1.000000000000000000, 0.8123765190705307671, 1.000000000000000000),
 ( 1.000000000000000000, 0.8190656277163975707, 1.000000000000000000),
 ( 1.000000000000000000, 0.8192366903512159348, 1.000000000000000000),
 ( 1.000000000000000000, 0.8126138454302893610, 1.000000000000000000),
 ( 1.000000000000000000, 0.8047712246031417660, 1.000000000000000000) ) ) 
 REPRESENTATION_ITEM ( '' )  SURFACE ( )  );
#18832 = VERTEX_POINT ( 'NONE', #5391 ) ;
#18833 = CARTESIAN_POINT ( 'NONE',  ( 145.0000000000000284, 0.000000000000000000, -90.00000000000000000 ) ) ;
#18834 = DIRECTION ( 'NONE',  ( 1.000000000000000000, 0.000000000000000000, 0.000000000000000000 ) ) ;
#18835 = ORIENTED_EDGE ( 'NONE', *, *, #17470, .T. ) ;
#18836 = CARTESIAN_POINT ( 'NONE',  ( 67.35000000000002274, -87.33333333333332860, 145.0000000000000000 ) ) ;
#18838 = AXIS2_PLACEMENT_3D ( 'NONE', #14443, #12788, #16355 ) ;
#18837 =( GEOMETRIC_REPRESENTATION_CONTEXT ( 3 ) GLOBAL_UNCERTAINTY_ASSIGNED_CONTEXT ( ( #1917 ) ) GLOBAL_UNIT_ASSIGNED_CONTEXT ( ( #22409, #12080, #22990 ) ) REPRESENTATION_CONTEXT ( 'NONE', 'WORKASPACE' ) );
#18839 = VERTEX_POINT ( 'NONE', #15412 ) ;
#18840 = VECTOR ( 'NONE', #12189, 1000.000000000000114 ) ;
#18841 = CIRCLE ( 'NONE', #14631, 2.649999999999985700 ) ;
#18842 = AXIS2_PLACEMENT_3D ( 'NONE', #9626, #18541, #5399 ) ;
#18843 = CARTESIAN_POINT ( 'NONE',  ( -285.2000000000013529, -89.99999999999897682, 26.98333333333330231 ) ) ;
#18844 = CIRCLE ( 'NONE', #17347, 5.249999999999949374 ) ;
#18845 = ORIENTED_EDGE ( 'NONE', *, *, #22699, .T. ) ;
#18846 = ADVANCED_FACE ( 'NONE', ( #18887 ), #6777, .T. ) ;
#18847 = FACE_OUTER_BOUND ( 'NONE', #19196, .T. ) ;
#18848 = DIRECTION ( 'NONE',  ( 0.000000000000000000, 1.000000000000000000, -3.491481338843133355E-15 ) ) ;
#18849 = EDGE_CURVE ( 'NONE', #8899, #8322, #13513, .T. ) ;
#18850 = EDGE_CURVE ( 'NONE', #20480, #16588, #16730, .T. ) ;
#18851 = VERTEX_POINT ( 'NONE', #5737 ) ;
#18852 = DIRECTION ( 'NONE',  ( 0.000000000000000000, 1.000000000000000000, -3.495664435217746987E-15 ) ) ;
#18853 = AXIS2_PLACEMENT_3D ( 'NONE', #16701, #1957, #2067 ) ;
#18854 = EDGE_LOOP ( 'NONE', ( #15783, #13160, #8248, #22774, #9028 ) ) ;
#18855 = CARTESIAN_POINT ( 'NONE',  ( 281.4928932188133217, -132.2000000000000455, 177.2000000000014097 ) ) ;
#18856 = EDGE_CURVE ( 'NONE', #9872, #1295, #14517, .T. ) ;
#18857 = CARTESIAN_POINT ( 'NONE',  ( -2.352990130084580066E-16, 8.660254037844390851, -7.422398894150034288 ) ) ;
#18858 = CARTESIAN_POINT ( 'NONE',  ( 100.0000000000000000, 249.9999999999999716, 125.0000000000000284 ) ) ;
#18859 = CARTESIAN_POINT ( 'NONE',  ( 281.4928932188134354, 267.8000000000000114, -144.9999999999999716 ) ) ;
#18860 = ORIENTED_EDGE ( 'NONE', *, *, #940, .F. ) ;
#18862 = CIRCLE ( 'NONE', #10423, 2.499999999999998668 ) ;
#18861 =( GEOMETRIC_REPRESENTATION_CONTEXT ( 3 ) GLOBAL_UNCERTAINTY_ASSIGNED_CONTEXT ( ( #7364 ) ) GLOBAL_UNIT_ASSIGNED_CONTEXT ( ( #18518, #14687, #2086 ) ) REPRESENTATION_CONTEXT ( 'NONE', 'WORKASPACE' ) );
#18863 = CARTESIAN_POINT ( 'NONE',  ( -280.9755899421581375, 269.7771650631953548, 145.4357337430840573 ) ) ;
#18864 = AXIS2_PLACEMENT_3D ( 'NONE', #20406, #18481, #20166 ) ;
#18865 = AXIS2_PLACEMENT_3D ( 'NONE', #8637, #6818, #21550 ) ;
#18866 = VECTOR ( 'NONE', #8901, 1000.000000000000000 ) ;
#18867 = VECTOR ( 'NONE', #12904, 1000.000000000000000 ) ;
#18869 = ORIENTED_EDGE ( 'NONE', *, *, #1190, .T. ) ;
#18868 = ORIENTED_EDGE ( 'NONE', *, *, #320, .F. ) ;
#18870 = DIRECTION ( 'NONE',  ( -1.000000000000000000, 0.000000000000000000, -6.982962677686266711E-15 ) ) ;
#18871 = DIRECTION ( 'NONE',  ( 0.000000000000000000, 0.000000000000000000, -1.000000000000000000 ) ) ;
#18872 = DIRECTION ( 'NONE',  ( -0.9510565162951510887, -0.3090169943749553894, 0.000000000000000000 ) ) ;
#18873 = CARTESIAN_POINT ( 'NONE',  ( -7.690461757479017101E-15, -129.2000000000000455, 0.000000000000000000 ) ) ;
#18874 = DIRECTION ( 'NONE',  ( -3.495664435217746987E-15, -1.000000000000000000, 0.000000000000000000 ) ) ;
#18875 = ORIENTED_EDGE ( 'NONE', *, *, #8374, .T. ) ;
#18876 = CARTESIAN_POINT ( 'NONE',  ( -4.000000000000000000, 2.309401076758498483, -3.433295621305379353 ) ) ;
#18878 = VECTOR ( 'NONE', #12206, 1000.000000000000000 ) ;
#18877 = AXIS2_PLACEMENT_3D ( 'NONE', #12869, #20172, #2053 ) ;
#18879 = PLANE ( 'NONE',  #6417 ) ;
#18880 = CARTESIAN_POINT ( 'NONE',  ( 280.0627246250093094, 273.0000000000000000, -145.3431883596742011 ) ) ;
#18881 = AXIS2_PLACEMENT_3D ( 'NONE', #12409, #3161, #7034 ) ;
#18882 = ORIENTED_EDGE ( 'NONE', *, *, #6361, .T. ) ;
#18883 = CIRCLE ( 'NONE', #8496, 2.055000000000000160 ) ;
#18884 = CARTESIAN_POINT ( 'NONE',  ( 99.99999999999987210, -132.2000000000003013, 177.2000000000014097 ) ) ;
#18885 = ADVANCED_FACE ( 'NONE', ( #11326 ), #8333, .F. ) ;
#18886 = ORIENTED_EDGE ( 'NONE', *, *, #7564, .F. ) ;
#18887 = FACE_OUTER_BOUND ( 'NONE', #14251, .T. ) ;
#18888 = CARTESIAN_POINT ( 'NONE',  ( 235.0000000000000284, -490.0000000000001137, -60.00000000000000000 ) ) ;
#18889 = EDGE_LOOP ( 'NONE', ( #21002, #6044, #20187, #5044, #18666, #6662, #21626, #8498, #3530, #9668, #8446, #20494 ) ) ;
#18890 = CARTESIAN_POINT ( 'NONE',  ( -312.2000000000014666, -129.2000000000000455, -146.4928932188134070 ) ) ;
#18891 = ADVANCED_FACE ( 'NONE', ( #6223 ), #14932, .T. ) ;
#18892 = VERTEX_POINT ( 'NONE', #9374 ) ;
#18893 = CARTESIAN_POINT ( 'NONE',  ( -160.0000000000000000, 0.000000000000000000, -100.0000000000000000 ) ) ;
#18894 = PLANE ( 'NONE',  #317 ) ;
#18895 = EDGE_CURVE ( 'NONE', #10923, #286, #1742, .T. ) ;
#18896 = DIRECTION ( 'NONE',  ( 1.000000000000000000, 0.000000000000000000, 0.000000000000000000 ) ) ;
#18897 = CARTESIAN_POINT ( 'NONE',  ( -44.99999999999995026, -59.79999999999968452, 105.0000000000002274 ) ) ;
#18898 = PLANE ( 'NONE',  #8834 ) ;
#18899 = DIRECTION ( 'NONE',  ( 0.000000000000000000, -1.000000000000000000, 0.000000000000000000 ) ) ;
#18900 = CARTESIAN_POINT ( 'NONE',  ( 7.499999999999999112, -4.330127018922205195, -1.000000000000000888 ) ) ;
#18901 = ADVANCED_FACE ( 'NONE', ( #20462 ), #7909, .F. ) ;
#18902 = ORIENTED_EDGE ( 'NONE', *, *, #19798, .F. ) ;
#18903 = EDGE_CURVE ( 'NONE', #17494, #16072, #11438, .T. ) ;
#18904 = PRESENTATION_STYLE_ASSIGNMENT (( #22879 ) ) ;
#18905 = CIRCLE ( 'NONE', #6558, 0.2500000000000002220 ) ;
#18906 = CARTESIAN_POINT ( 'NONE',  ( 194.7499999999997442, -209.9999999999996874, 30.00000000000675726 ) ) ;
#18907 = FACE_OUTER_BOUND ( 'NONE', #19322, .T. ) ;
#18908 = ORIENTED_EDGE ( 'NONE', *, *, #11804, .F. ) ;
#18909 = AXIS2_PLACEMENT_3D ( 'NONE', #13780, #21455, #17378 ) ;
#18910 = CIRCLE ( 'NONE', #5430, 7.500000000000000888 ) ;
#18911 = EDGE_LOOP ( 'NONE', ( #13187, #22510, #20123 ) ) ;
#18912 = CARTESIAN_POINT ( 'NONE',  ( 0.000000000000000000, 0.000000000000000000, 100.0000000000000000 ) ) ;
#18913 = DIRECTION ( 'NONE',  ( 1.000000000000000000, 0.000000000000000000, 0.000000000000000000 ) ) ;
#18914 = DIRECTION ( 'NONE',  ( 1.000000000000000000, 0.000000000000000000, 0.000000000000000000 ) ) ;
#18915 = ORIENTED_EDGE ( 'NONE', *, *, #2601, .T. ) ;
#18916 = DIRECTION ( 'NONE',  ( 0.6568457881071740889, 0.2618274444092085762, -0.7071067811865532349 ) ) ;
#18917 = DIRECTION ( 'NONE',  ( -0.000000000000000000, -0.000000000000000000, -1.000000000000000000 ) ) ;
#18918 = B_SPLINE_CURVE_WITH_KNOTS ( 'NONE', 3,
 ( #16620, #9369, #3441, #22141, #14455, #12666, #20325, #10858, #18183, #1627, #9008, #16372, #23720, #7175, #14567, #21905, #10961, #18283, #18880, #17330 ),
 .UNSPECIFIED., .F., .F.,
 ( 4, 2, 2, 2, 2, 2, 2, 2, 2, 4 ),
 ( 0.000000000000000000, 0.001035985217005741836, 0.002071970434011483671, 0.003107955651017225290, 0.003625948259520141419, 0.004143940868023057549, 0.005179926085028801336, 0.006215911302034544256, 0.007251896519040288043, 0.008287881736046031830 ),
 .UNSPECIFIED. ) ;
#18919 = FACE_OUTER_BOUND ( 'NONE', #15334, .T. ) ;
#18920 = ORIENTED_EDGE ( 'NONE', *, *, #14212, .F. ) ;
#18921 = CARTESIAN_POINT ( 'NONE',  ( 280.1245861693739130, 272.9663417894421968, 145.6816199723481304 ) ) ;
#18922 = LINE ( 'NONE', #15205, #1103 ) ;
#18923 = CARTESIAN_POINT ( 'NONE',  ( 1.499998969197076093, 9.887698300110391969, 200.0000060000000133 ) ) ;
#18924 = EDGE_LOOP ( 'NONE', ( #8569, #13316, #477, #14462 ) ) ;
#18925 = DIRECTION ( 'NONE',  ( -1.000000000000000000, -0.000000000000000000, -0.000000000000000000 ) ) ;
#18926 = DIRECTION ( 'NONE',  ( -0.000000000000000000, 0.000000000000000000, 1.000000000000000000 ) ) ;
#18927 = FACE_OUTER_BOUND ( 'NONE', #15348, .T. ) ;
#18928 = FACE_OUTER_BOUND ( 'NONE', #2416, .T. ) ;
#18929 = ORIENTED_EDGE ( 'NONE', *, *, #20619, .T. ) ;
#18931 = ORIENTED_EDGE ( 'NONE', *, *, #9436, .T. ) ;
#18930 = EDGE_CURVE ( 'NONE', #10712, #9953, #10264, .T. ) ;
#18932 = EDGE_CURVE ( 'NONE', #15661, #6073, #14139, .T. ) ;
#18933 = CARTESIAN_POINT ( 'NONE',  ( 0.000000000000000000, -127.0000000000000568, 150.2000000000013813 ) ) ;
#18934 = DIRECTION ( 'NONE',  ( -0.000000000000000000, -0.000000000000000000, 1.000000000000000000 ) ) ;
#18935 = EDGE_CURVE ( 'NONE', #5442, #18735, #20833, .T. ) ;
#18936 = ORIENTED_EDGE ( 'NONE', *, *, #4596, .T. ) ;
#18937 = CYLINDRICAL_SURFACE ( 'NONE', #6338, 5.199999999999982414 ) ;
#18938 = DIRECTION ( 'NONE',  ( 0.5877852522924826850, -0.8090169943749405679, 0.000000000000000000 ) ) ;
#18939 = ORIENTED_EDGE ( 'NONE', *, *, #12033, .T. ) ;
#18940 = CARTESIAN_POINT ( 'NONE',  ( 70.00000000000000000, -112.6666666666666714, 0.000000000000000000 ) ) ;
#18941 = ORIENTED_EDGE ( 'NONE', *, *, #10549, .T. ) ;
#18942 = CYLINDRICAL_SURFACE ( 'NONE', #12979, 2.500000000000002220 ) ;
#18943 = CARTESIAN_POINT ( 'NONE',  ( 5.000000000000000000, 4.685197434473814759, -5.637851296924623057E-15 ) ) ;
#18944 = EDGE_LOOP ( 'NONE', ( #16721, #151, #11128, #10529 ) ) ;
#18945 = ORIENTED_EDGE ( 'NONE', *, *, #23770, .F. ) ;
#18946 = CARTESIAN_POINT ( 'NONE',  ( 0.000000000000000000, 0.000000000000000000, 0.000000000000000000 ) ) ;
#18947 = CARTESIAN_POINT ( 'NONE',  ( 1.654252653721905331, 3.663718938583014229, -0.01223254789873410957 ) ) ;
#18948 = CARTESIAN_POINT ( 'NONE',  ( -19.87444003266269021, -1015.254521007281141, -145.0000000000001421 ) ) ;
#18949 = CARTESIAN_POINT ( 'NONE',  ( 282.6054396500288703, 272.3132312761072171, 145.4975000228326678 ) ) ;
#18950 = CARTESIAN_POINT ( 'NONE',  ( 21.69578997558837585, -987.4712331462250177, 145.0000119999999697 ) ) ;
#18951 = FACE_OUTER_BOUND ( 'NONE', #20940, .T. ) ;
#18952 = DIRECTION ( 'NONE',  ( 1.000000000000000000, 0.000000000000000000, 0.000000000000000000 ) ) ;
#18953 = ORIENTED_EDGE ( 'NONE', *, *, #21208, .T. ) ;
#18954 = DIRECTION ( 'NONE',  ( -0.000000000000000000, -0.000000000000000000, 1.000000000000000000 ) ) ;
#18955 = CARTESIAN_POINT ( 'NONE',  ( -3.093533885184598375, -6.874201416485457017, -7.446478553994068328 ) ) ;
#18956 = VERTEX_POINT ( 'NONE', #13265 ) ;
#18957 = EDGE_CURVE ( 'NONE', #8986, #17768, #4154, .T. ) ;
#18958 = CARTESIAN_POINT ( 'NONE',  ( -136.9913212208051903, -1072.514673757700621, -29.83733181946746882 ) ) ;
#18959 = LINE ( 'NONE', #16049, #9560 ) ;
#18960 =( REPRESENTATION_RELATIONSHIP ('NONE','NONE', #10127, #5587 ) REPRESENTATION_RELATIONSHIP_WITH_TRANSFORMATION ( #20432 )SHAPE_REPRESENTATION_RELATIONSHIP( ) );
#18961 = EDGE_LOOP ( 'NONE', ( #9387, #19100, #2926, #5565 ) ) ;
#18962 = CARTESIAN_POINT ( 'NONE',  ( -134.8618744214600440, -1076.402150461713063, 31.66065886938995533 ) ) ;
#18963 = ORIENTED_EDGE ( 'NONE', *, *, #2940, .F. ) ;
#18964 = DIRECTION ( 'NONE',  ( 1.000000000000000000, 0.000000000000000000, 0.000000000000000000 ) ) ;
#18965 = CARTESIAN_POINT ( 'NONE',  ( 283.9159870726004442, 271.2379565153281078, -145.8082263737022117 ) ) ;
#18966 = EDGE_LOOP ( 'NONE', ( #22188, #3260, #8608, #23374 ) ) ;
#18967 = DIRECTION ( 'NONE',  ( 0.000000000000000000, 0.000000000000000000, -1.000000000000000000 ) ) ;
#18968 = DIRECTION ( 'NONE',  ( -1.110223024625155594E-14, 0.000000000000000000, -1.000000000000000000 ) ) ;
#18969 = ORIENTED_EDGE ( 'NONE', *, *, #13281, .T. ) ;
#18970 = FACE_OUTER_BOUND ( 'NONE', #3309, .T. ) ;
#18971 = ORIENTED_EDGE ( 'NONE', *, *, #21673, .T. ) ;
#18972 = CARTESIAN_POINT ( 'NONE',  ( 4.211140560182196957, 2.431303136016536470, -3.745885042887433514 ) ) ;
#18973 = CARTESIAN_POINT ( 'NONE',  ( 2.500000000000000444, 7.216878364870322748, -7.063244554130000630 ) ) ;
#18974 = EDGE_CURVE ( 'NONE', #23519, #19241, #5856, .T. ) ;
#18975 = VECTOR ( 'NONE', #9397, 1000.000000000000000 ) ;
#18976 = DIRECTION ( 'NONE',  ( -0.000000000000000000, -1.000000000000000000, -3.495664435217746987E-15 ) ) ;
#18977 = DIRECTION ( 'NONE',  ( 0.000000000000000000, -1.000000000000000000, 0.000000000000000000 ) ) ;
#18978 = ORIENTED_EDGE ( 'NONE', *, *, #790, .F. ) ;
#18979 = CARTESIAN_POINT ( 'NONE',  ( 50.00000000000000000, 0.000000000000000000, 0.000000000000000000 ) ) ;
#18981 = ORIENTED_EDGE ( 'NONE', *, *, #14597, .T. ) ;
#18980 = ORIENTED_EDGE ( 'NONE', *, *, #14744, .F. ) ;
#18982 = ADVANCED_FACE ( 'NONE', ( #2463 ), #18755, .F. ) ;
#18983 = DIRECTION ( 'NONE',  ( -5.050510105632271307E-15, 4.822252111914687128E-15, -1.000000000000000000 ) ) ;
#18984 = DIRECTION ( 'NONE',  ( 0.000000000000000000, 0.000000000000000000, -1.000000000000000000 ) ) ;
#18985 = CARTESIAN_POINT ( 'NONE',  ( 131.5594662024485899, 81.95796442703947093, -29.34624901867147884 ) ) ;
#18986 = ADVANCED_FACE ( 'NONE', ( #17088, #7789, #22505, #5974, #22625, #13381, #20693 ), #19472, .F. ) ;
#18987 = CARTESIAN_POINT ( 'NONE',  ( 0.000000000000000000, 0.000000000000000000, 0.000000000000000000 ) ) ;
#18988 = DIRECTION ( 'NONE',  ( 0.000000000000000000, 1.110223024625156540E-16, -1.000000000000000000 ) ) ;
#18989 = VERTEX_POINT ( 'NONE', #8519 ) ;
#18990 = EDGE_CURVE ( 'NONE', #17401, #7876, #16952, .T. ) ;
#18991 = VECTOR ( 'NONE', #5190, 1000.000000000000114 ) ;
#18992 = DIRECTION ( 'NONE',  ( 0.000000000000000000, 0.000000000000000000, 1.000000000000000000 ) ) ;
#18993 = DIRECTION ( 'NONE',  ( -0.9423651898111408132, -0.3345860861306287348, 6.982962677686266711E-15 ) ) ;
#18994 = CARTESIAN_POINT ( 'NONE',  ( 124.2727838502227797, -1092.635313011623111, 32.48389983298808659 ) ) ;
#18995 = ITEM_DEFINED_TRANSFORMATION ( 'NONE', 'NONE', #11206,  #11210 ) ;
#18996 = ORIENTED_EDGE ( 'NONE', *, *, #8611, .T. ) ;
#18997 = CARTESIAN_POINT ( 'NONE',  ( 40.00000000000000000, 100.0000000000000000, -147.2000000000005571 ) ) ;
#18998 = VERTEX_POINT ( 'NONE', #17554 ) ;
#18999 = CARTESIAN_POINT ( 'NONE',  ( 0.000000000000000000, 0.000000000000000000, -100.0000000000000000 ) ) ;
#19000 = LINE ( 'NONE', #549, #225 ) ;
#19001 = ORIENTED_EDGE ( 'NONE', *, *, #21833, .T. ) ;
#19002 = CARTESIAN_POINT ( 'NONE',  ( -107.6499999999999631, -29.99999999999998579, 0.000000000000000000 ) ) ;
#19003 = ORIENTED_EDGE ( 'NONE', *, *, #7871, .T. ) ;
#19004 = DIRECTION ( 'NONE',  ( -0.000000000000000000, -0.000000000000000000, -1.000000000000000000 ) ) ;
#19005 = DIRECTION ( 'NONE',  ( 1.000000000000000000, 0.000000000000000000, 0.000000000000000000 ) ) ;
#19006 = DIRECTION ( 'NONE',  ( 1.000000000000000000, 0.000000000000000000, 0.000000000000000000 ) ) ;
#19007 = DIRECTION ( 'NONE',  ( -0.000000000000000000, -0.000000000000000000, 1.000000000000000000 ) ) ;
#19008 = CARTESIAN_POINT ( 'NONE',  ( -79.99999999999994316, -56.79999999999918714, 250.0000000000000000 ) ) ;
#19009 = DIRECTION ( 'NONE',  ( -1.000000000000000000, -0.000000000000000000, -0.000000000000000000 ) ) ;
#19010 = DIRECTION ( 'NONE',  ( 0.000000000000000000, -1.000000000000000000, 0.000000000000000000 ) ) ;
#19011 = ORIENTED_EDGE ( 'NONE', *, *, #16608, .F. ) ;
#19012 = EDGE_CURVE ( 'NONE', #22939, #17429, #19267, .T. ) ;
#19013 = EDGE_CURVE ( 'NONE', #1663, #12205, #1134, .T. ) ;
#19014 = DIRECTION ( 'NONE',  ( -0.000000000000000000, -0.000000000000000000, 1.000000000000000000 ) ) ;
#19015 = FACE_OUTER_BOUND ( 'NONE', #21637, .T. ) ;
#19016 = VERTEX_POINT ( 'NONE', #4880 ) ;
#19017 = ORIENTED_EDGE ( 'NONE', *, *, #20454, .T. ) ;
#19018 = DIRECTION ( 'NONE',  ( -1.000000000000000000, 0.000000000000000000, 0.000000000000000000 ) ) ;
#19019 = CARTESIAN_POINT ( 'NONE',  ( 146.0000000000002558, -210.0000000000003411, -32.05499999999356930 ) ) ;
#19020 = ADVANCED_FACE ( 'NONE', ( #8166 ), #21187, .F. ) ;
#19021 = DIRECTION ( 'NONE',  ( 0.000000000000000000, 0.000000000000000000, 1.000000000000000000 ) ) ;
#19022 = AXIS2_PLACEMENT_3D ( 'NONE', #21615, #5071, #12591 ) ;
#19023 = ADVANCED_FACE ( 'NONE', ( #6693 ), #8383, .F. ) ;
#19024 = AXIS2_PLACEMENT_3D ( 'NONE', #11224, #5750, #3675 ) ;
#19025 = ORIENTED_EDGE ( 'NONE', *, *, #17519, .F. ) ;
#19026 = DIRECTION ( 'NONE',  ( 0.000000000000000000, 0.000000000000000000, 1.000000000000000000 ) ) ;
#19027 = CARTESIAN_POINT ( 'NONE',  ( 281.4928932188133786, -127.0000000000000568, -150.2000000000013245 ) ) ;
#19028 = ADVANCED_FACE ( 'NONE', ( #21306 ), #4399, .F. ) ;
#19029 = CARTESIAN_POINT ( 'NONE',  ( 2.500000000000000000, 0.000000000000000000, 0.000000000000000000 ) ) ;
#19030 = ORIENTED_EDGE ( 'NONE', *, *, #18781, .T. ) ;
#19031 = CARTESIAN_POINT ( 'NONE',  ( -285.2000000000000455, 267.7999999999999545, 146.4928932188134638 ) ) ;
#19032 = CARTESIAN_POINT ( 'NONE',  ( -3.000000000000002665, 2.936090700955779358E-15, 23.97500000000000142 ) ) ;
#19033 = ADVANCED_FACE ( 'NONE', ( #15649 ), #12287, .F. ) ;
#19034 = DIRECTION ( 'NONE',  ( -0.000000000000000000, -0.000000000000000000, 1.000000000000000000 ) ) ;
#19035 = ORIENTED_EDGE ( 'NONE', *, *, #23777, .T. ) ;
#19036 = CARTESIAN_POINT ( 'NONE',  ( -312.2000000000014666, -132.2000000000000455, -146.4928932188134070 ) ) ;
#19037 = CONTEXT_DEPENDENT_SHAPE_REPRESENTATION ( #596, #23470 ) ;
#19038 = DIRECTION ( 'NONE',  ( -1.000000000000000000, 0.000000000000000000, 0.000000000000000000 ) ) ;
#19039 = DIRECTION ( 'NONE',  ( -1.000000000000000000, 1.408839003528726857E-14, 6.982962677686266711E-15 ) ) ;
#19040 = CARTESIAN_POINT ( 'NONE',  ( 45.00000000000004974, -59.79999999999965610, 102.3500000000002359 ) ) ;
#19041 = AXIS2_PLACEMENT_3D ( 'NONE', #10969, #1401, #17952 ) ;
#19042 = ORIENTED_EDGE ( 'NONE', *, *, #20545, .F. ) ;
#19043 = CONICAL_SURFACE ( 'NONE', #7113, 2.055000000000001492, 0.7853981633974633780 ) ;
#19044 = ORIENTED_EDGE ( 'NONE', *, *, #22574, .T. ) ;
#19045 = CYLINDRICAL_SURFACE ( 'NONE', #11505, 145.0000000000000284 ) ;
#19046 = DIRECTION ( 'NONE',  ( 1.000000000000000000, 0.000000000000000000, 0.000000000000000000 ) ) ;
#19047 = AXIS2_PLACEMENT_3D ( 'NONE', #7840, #11488, #22439 ) ;
#19048 = EDGE_CURVE ( 'NONE', #18546, #6258, #10469, .T. ) ;
#19049 = VERTEX_POINT ( 'NONE', #17808 ) ;
#19050 = DIRECTION ( 'NONE',  ( 0.000000000000000000, -1.000000000000000000, 3.700743415417187942E-15 ) ) ;
#19051 = CARTESIAN_POINT ( 'NONE',  ( -126.9531799701279766, 88.92639545932793510, 28.11170275877340075 ) ) ;
#19052 = EDGE_LOOP ( 'NONE', ( #13710, #9907, #12063, #10193 ) ) ;
#19053 = EDGE_CURVE ( 'NONE', #19892, #11790, #18862, .T. ) ;
#19054 = DIRECTION ( 'NONE',  ( 3.700743415417189520E-15, 1.000000000000000000, 0.000000000000000000 ) ) ;
#19055 = CIRCLE ( 'NONE', #18281, 5.200000000000028599 ) ;
#19056 = ORIENTED_EDGE ( 'NONE', *, *, #23380, .F. ) ;
#19057 = AXIS2_PLACEMENT_3D ( 'NONE', #1984, #14328, #7314 ) ;
#19058 = ADVANCED_FACE ( 'NONE', ( #2582 ), #888, .F. ) ;
#19059 = DIRECTION ( 'NONE',  ( -1.000000000000000000, 0.000000000000000000, 0.000000000000000000 ) ) ;
#19060 = ADVANCED_FACE ( 'NONE', ( #15760 ), #23105, .T. ) ;
#19061 = DIRECTION ( 'NONE',  ( 0.000000000000000000, 0.000000000000000000, 1.000000000000000000 ) ) ;
#19062 = EDGE_LOOP ( 'NONE', ( #13062, #6792, #14114 ) ) ;
#19063 = ORIENTED_EDGE ( 'NONE', *, *, #22909, .T. ) ;
#19064 = DIRECTION ( 'NONE',  ( 0.6964005597823107463, -0.7176533009294140397, 6.982962677686265922E-15 ) ) ;
#19065 = MECHANICAL_DESIGN_GEOMETRIC_PRESENTATION_REPRESENTATION (  '', ( #17925 ), #5204 ) ;
#19066 = AXIS2_PLACEMENT_3D ( 'NONE', #16368, #14565, #11205 ) ;
#19067 = LINE ( 'NONE', #7742, #3842 ) ;
#19068 = CARTESIAN_POINT ( 'NONE',  ( 0.2500000000000002220, 0.000000000000000000, 4.250000000000000000 ) ) ;
#19069 = DIRECTION ( 'NONE',  ( 0.000000000000000000, 0.000000000000000000, -1.000000000000000000 ) ) ;
#19070 = FACE_OUTER_BOUND ( 'NONE', #21924, .T. ) ;
#19071 = ORIENTED_EDGE ( 'NONE', *, *, #15638, .F. ) ;
#19072 = DIRECTION ( 'NONE',  ( 0.000000000000000000, -0.4999999999999992228, 0.8660254037844390407 ) ) ;
#19073 = AXIS2_PLACEMENT_3D ( 'NONE', #23753, #14487, #5289 ) ;
#19074 = EDGE_LOOP ( 'NONE', ( #15360, #16115 ) ) ;
#19075 = DIRECTION ( 'NONE',  ( -1.000000000000000000, -0.000000000000000000, -0.000000000000000000 ) ) ;
#19076 = CARTESIAN_POINT ( 'NONE',  ( 3.861362476283255685, 2.629030857715988656, -3.671615880910370500 ) ) ;
#19077 = MECHANICAL_DESIGN_GEOMETRIC_PRESENTATION_REPRESENTATION (  '', ( #10792 ), #588 ) ;
#19078 = ORIENTED_EDGE ( 'NONE', *, *, #18930, .T. ) ;
#19079 = AXIS2_PLACEMENT_3D ( 'NONE', #14746, #3598, #20151 ) ;
#19080 = DIRECTION ( 'NONE',  ( -1.000000000000000000, 0.000000000000000000, -0.000000000000000000 ) ) ;
#19081 = EDGE_LOOP ( 'NONE', ( #3698, #18487 ) ) ;
#19082 = CARTESIAN_POINT ( 'NONE',  ( -31.74999999999995737, 0.000000000000000000, 0.000000000000000000 ) ) ;
#19083 = CARTESIAN_POINT ( 'NONE',  ( 283.4314821058791836, 271.7107452280323514, -145.6845057130644818 ) ) ;
#19084 = VERTEX_POINT ( 'NONE', #22976 ) ;
#19085 = EDGE_CURVE ( 'NONE', #20130, #7169, #22861, .T. ) ;
#19086 = CARTESIAN_POINT ( 'NONE',  ( -280.4976310729379065, 269.6958543268121957, 146.0927021017107563 ) ) ;
#19087 = CYLINDRICAL_SURFACE ( 'NONE', #6522, 5.249999999999942268 ) ;
#19088 = EDGE_CURVE ( 'NONE', #12339, #18758, #4757, .T. ) ;
#19089 = ORIENTED_EDGE ( 'NONE', *, *, #19425, .F. ) ;
#19090 =( REPRESENTATION_RELATIONSHIP ('NONE','NONE', #10127, #4684 ) REPRESENTATION_RELATIONSHIP_WITH_TRANSFORMATION ( #819 )SHAPE_REPRESENTATION_RELATIONSHIP( ) );
#19091 = UNCERTAINTY_MEASURE_WITH_UNIT (LENGTH_MEASURE( 1.000000000000000082E-05 ), #13364, 'distance_accuracy_value', 'NONE');
#19092 = ADVANCED_FACE ( 'NONE', ( #12172 ), #10104, .T. ) ;
#19093 = PLANE ( 'NONE',  #7556 ) ;
#19094 = CARTESIAN_POINT ( 'NONE',  ( 65.00000000000004263, -52.79999999999959925, 65.00000000000018474 ) ) ;
#19095 = DIRECTION ( 'NONE',  ( 0.000000000000000000, 0.000000000000000000, 1.000000000000000000 ) ) ;
#19096 = AXIS2_PLACEMENT_3D ( 'NONE', #8103, #2766, #4818 ) ;
#19097 = VECTOR ( 'NONE', #13432, 1000.000000000000000 ) ;
#19098 = LINE ( 'NONE', #19336, #11946 ) ;
#19099 = B_SPLINE_CURVE_WITH_KNOTS ( 'NONE', 3,
 ( #6947, #1012, #7053, #14099, #10340, #14211 ),
 .UNSPECIFIED., .F., .F.,
 ( 4, 2, 4 ),
 ( 0.004444412883774326306, 0.006655097293744431999, 0.008865781703714537693 ),
 .UNSPECIFIED. ) ;
#19100 = ORIENTED_EDGE ( 'NONE', *, *, #12931, .T. ) ;
#19101 = DIRECTION ( 'NONE',  ( 0.000000000000000000, 0.000000000000000000, 1.000000000000000000 ) ) ;
#19102 = PRODUCT_DEFINITION_SHAPE ( 'NONE', 'NONE',  #23867 ) ;
#19104 = VERTEX_POINT ( 'NONE', #1370 ) ;
#19103 = ORIENTED_EDGE ( 'NONE', *, *, #10986, .F. ) ;
#19105 = DIRECTION ( 'NONE',  ( 4.862939117679700002E-15, -5.011346215908450209E-15, -1.000000000000000000 ) ) ;
#19106 = LINE ( 'NONE', #13842, #15444 ) ;
#19107 = VECTOR ( 'NONE', #6967, 1000.000000000000114 ) ;
#19108 = DIRECTION ( 'NONE',  ( -0.000000000000000000, -0.000000000000000000, 1.000000000000000000 ) ) ;
#19109 = B_SPLINE_CURVE_WITH_KNOTS ( 'NONE', 3,
 ( #16961, #16833, #290, #426, #14919, #13143, #20561, #16719, #9841, #7646, #22384, #20816, #18985, #17198, #14800, #173, #7527, #20450, #18623, #11915, #2913, #8018, #2568, #10312, #15397, #17656, #17539, #4867 ),
 .UNSPECIFIED., .F., .F.,
 ( 4, 2, 2, 2, 2, 2, 2, 2, 2, 2, 2, 2, 2, 4 ),
 ( 0.007862850516742132811, 0.008354729399060706330, 0.008846608281379278113, 0.009830366046016423415, 0.01032224492833497959, 0.01081412381065353749, 0.01130600269297209540, 0.01179788157529065157, 0.01278163933992775350, 0.01327351822224632702, 0.01376539710456489880, 0.01425727598688347059, 0.01474915486920204237, 0.01573291263383914604 ),
 .UNSPECIFIED. ) ;
#19110 = CARTESIAN_POINT ( 'NONE',  ( 282.1132285165672329, 268.3679143846943020, 146.2440776823445958 ) ) ;
#19111 = CIRCLE ( 'NONE', #14897, 2.500000000000002220 ) ;
#19112 = FACE_OUTER_BOUND ( 'NONE', #7085, .T. ) ;
#19113 = ORIENTED_EDGE ( 'NONE', *, *, #5493, .T. ) ;
#19114 = VECTOR ( 'NONE', #17555, 1000.000000000000000 ) ;
#19115 = CARTESIAN_POINT ( 'NONE',  ( -1.999999999999999556, 3.464101615137754830, -3.142992957459232795 ) ) ;
#19116 = DIRECTION ( 'NONE',  ( 0.000000000000000000, 0.000000000000000000, 1.000000000000000000 ) ) ;
#19117 = LINE ( 'NONE', #22621, #380 ) ;
#19118 = ORIENTED_EDGE ( 'NONE', *, *, #11074, .F. ) ;
#19119 = EDGE_CURVE ( 'NONE', #4309, #13384, #18696, .T. ) ;
#19120 = DIRECTION ( 'NONE',  ( -1.000000000000000000, 1.408839003528726857E-14, 6.982962677686266711E-15 ) ) ;
#19121 = EDGE_LOOP ( 'NONE', ( #73, #7755, #22393, #9657 ) ) ;
#19122 = DIRECTION ( 'NONE',  ( 0.000000000000000000, 0.000000000000000000, -1.000000000000000000 ) ) ;
#19123 = DIRECTION ( 'NONE',  ( 1.000000000000000000, 0.000000000000000000, 0.000000000000000000 ) ) ;
#19124 = EDGE_LOOP ( 'NONE', ( #6597, #15863, #22961, #12592 ) ) ;
#19125 = CIRCLE ( 'NONE', #22588, 2.500000000000002220 ) ;
#19126 = LINE ( 'NONE', #22765, #14851 ) ;
#19127 = ORIENTED_EDGE ( 'NONE', *, *, #19927, .T. ) ;
#19128 = DIRECTION ( 'NONE',  ( 1.000000000000000000, 0.000000000000000000, 0.000000000000000000 ) ) ;
#19129 = CYLINDRICAL_SURFACE ( 'NONE', #16130, 8.000000000000000000 ) ;
#19130 = FACE_BOUND ( 'NONE', #6028, .T. ) ;
#19131 = LINE ( 'NONE', #10112, #1701 ) ;
#19132 = CARTESIAN_POINT ( 'NONE',  ( -105.0000000000000000, -29.99999999999998579, 3.000000000000000000 ) ) ;
#19133 = CARTESIAN_POINT ( 'NONE',  ( 0.000000000000000000, -1000.000000000000000, -150.0000000000000000 ) ) ;
#19134 = CARTESIAN_POINT ( 'NONE',  ( 2.500000000000000000, 0.000000000000000000, 0.000000000000000000 ) ) ;
#19135 = VERTEX_POINT ( 'NONE', #16786 ) ;
#19136 =( NAMED_UNIT ( * ) SI_UNIT ( $, .STERADIAN. ) SOLID_ANGLE_UNIT ( ) );
#19137 = LINE ( 'NONE', #5869, #16890 ) ;
#19138 = CARTESIAN_POINT ( 'NONE',  ( 126.7787238282394924, 77.44864885511604768, 30.00000000000641975 ) ) ;
#19139 = ORIENTED_EDGE ( 'NONE', *, *, #19483, .T. ) ;
#19140 = ORIENTED_EDGE ( 'NONE', *, *, #4437, .T. ) ;
#19141 = CYLINDRICAL_SURFACE ( 'NONE', #2264, 2.649999999999999467 ) ;
#19142 = DIRECTION ( 'NONE',  ( 1.000000000000000000, -0.000000000000000000, -0.000000000000000000 ) ) ;
#19143 =( NAMED_UNIT ( * ) SI_UNIT ( $, .STERADIAN. ) SOLID_ANGLE_UNIT ( ) );
#19144 = CARTESIAN_POINT ( 'NONE',  ( 287.4000000000013415, -132.2000000000000455, 146.4928932188134638 ) ) ;
#19145 = CARTESIAN_POINT ( 'NONE',  ( 131.6538433078035268, 81.80629369879993362, 31.11671059283535712 ) ) ;
#19146 = LINE ( 'NONE', #22890, #14765 ) ;
#19147 = CARTESIAN_POINT ( 'NONE',  ( -49.99999999999997158, 1.525580655599899097E-29, 3.000000000000000000 ) ) ;
#19148 = ORIENTED_EDGE ( 'NONE', *, *, #15767, .T. ) ;
#19149 = EDGE_CURVE ( 'NONE', #6073, #15661, #22352, .T. ) ;
#19150 = DIRECTION ( 'NONE',  ( -0.000000000000000000, 0.000000000000000000, -1.000000000000000000 ) ) ;
#19151 = CARTESIAN_POINT ( 'NONE',  ( 0.2500000000000002220, 0.000000000000000000, 0.000000000000000000 ) ) ;
#19152 =( NAMED_UNIT ( * ) SI_UNIT ( $, .STERADIAN. ) SOLID_ANGLE_UNIT ( ) );
#19153 = EDGE_CURVE ( 'NONE', #9210, #4056, #15785, .T. ) ;
#19154 = ORIENTED_EDGE ( 'NONE', *, *, #4589, .T. ) ;
#19155 = VECTOR ( 'NONE', #5437, 1000.000000000000000 ) ;
#19156 = CARTESIAN_POINT ( 'NONE',  ( 280.2840560642350738, 269.9696999999999889, -145.1244266425809144 ) ) ;
#19157 = APPLICATION_PROTOCOL_DEFINITION ( 'draft international standard', 'automotive_design', 1998, #8923 ) ;
#19158 = DIRECTION ( 'NONE',  ( -0.6964005597823108573, 0.7176533009294141507, -6.982962677686267499E-15 ) ) ;
#19159 = VECTOR ( 'NONE', #20385, 1000.000000000000114 ) ;
#19160 = EDGE_CURVE ( 'NONE', #6579, #11264, #22388, .T. ) ;
#19162 = EDGE_CURVE ( 'NONE', #21974, #22922, #12968, .T. ) ;
#19161 = CARTESIAN_POINT ( 'NONE',  ( 0.000000000000000000, 0.000000000000000000, -90.00000000000000000 ) ) ;
#19163 = FACE_OUTER_BOUND ( 'NONE', #17648, .T. ) ;
#19164 = UNCERTAINTY_MEASURE_WITH_UNIT (LENGTH_MEASURE( 1.000000000000000082E-05 ), #12282, 'distance_accuracy_value', 'NONE');
#19165 = ORIENTED_EDGE ( 'NONE', *, *, #17010, .T. ) ;
#19166 = ORIENTED_EDGE ( 'NONE', *, *, #23653, .F. ) ;
#19167 = CARTESIAN_POINT ( 'NONE',  ( 24.99999999999999645, 2.463415629691065208E-15, 145.0000059999999849 ) ) ;
#19168 = FACE_OUTER_BOUND ( 'NONE', #10481, .T. ) ;
#19169 = ORIENTED_EDGE ( 'NONE', *, *, #17688, .F. ) ;
#19170 = EDGE_CURVE ( 'NONE', #3985, #711, #16205, .T. ) ;
#19171 = VECTOR ( 'NONE', #10512, 1000.000000000000000 ) ;
#19172 = EDGE_LOOP ( 'NONE', ( #17553, #21162, #21534, #3721 ) ) ;
#19173 = CYLINDRICAL_SURFACE ( 'NONE', #9874, 25.00000000000000000 ) ;
#19174 = LINE ( 'NONE', #2637, #14950 ) ;
#19175 = ORIENTED_EDGE ( 'NONE', *, *, #16670, .F. ) ;
#19176 = AXIS2_PLACEMENT_3D ( 'NONE', #16967, #6084, #6216 ) ;
#19177 = FACE_OUTER_BOUND ( 'NONE', #19491, .T. ) ;
#19178 = AXIS2_PLACEMENT_3D ( 'NONE', #7104, #18436, #10759 ) ;
#19179 = AXIS2_PLACEMENT_3D ( 'NONE', #9284, #22054, #12696 ) ;
#19180 = ORIENTED_EDGE ( 'NONE', *, *, #6987, .T. ) ;
#19181 = CARTESIAN_POINT ( 'NONE',  ( 90.00000000000000000, 95.00000000000000000, 3.000000000000000000 ) ) ;
#19182 = DIRECTION ( 'NONE',  ( 1.000000000000000000, 0.000000000000000000, -0.000000000000000000 ) ) ;
#19183 = ORIENTED_EDGE ( 'NONE', *, *, #2658, .T. ) ;
#19184 = ORIENTED_EDGE ( 'NONE', *, *, #13392, .F. ) ;
#19185 = CARTESIAN_POINT ( 'NONE',  ( 1.390230914382191596, 4.043987460488659202, -3.502507215260488582 ) ) ;
#19186 = ADVANCED_FACE ( 'NONE', ( #1803 ), #9196, .T. ) ;
#19187 = CARTESIAN_POINT ( 'NONE',  ( -7.640563834021360018E-16, -9.147862274876560562, -8.047472243342937759 ) ) ;
#19188 = EDGE_CURVE ( 'NONE', #20673, #3845, #9322, .T. ) ;
#19189 = DIRECTION ( 'NONE',  ( 1.000000000000000000, 3.495664435217746987E-15, 0.000000000000000000 ) ) ;
#19190 = ORIENTED_EDGE ( 'NONE', *, *, #14322, .T. ) ;
#19191 = EDGE_CURVE ( 'NONE', #22443, #2736, #20401, .T. ) ;
#19192 = CARTESIAN_POINT ( 'NONE',  ( -4.197393957002303999, -0.8151795401431414234, -3.503767560748935139 ) ) ;
#19193 =( NAMED_UNIT ( * ) SI_UNIT ( $, .STERADIAN. ) SOLID_ANGLE_UNIT ( ) );
#19194 = AXIS2_PLACEMENT_3D ( 'NONE', #9862, #9621, #17348 ) ;
#19195 = ADVANCED_FACE ( 'NONE', ( #608 ), #6368, .F. ) ;
#19196 = EDGE_LOOP ( 'NONE', ( #11463, #16843, #20147, #4022 ) ) ;
#19197 = PRODUCT_DEFINITION ( 'UNKNOWN', '', #2305, #18681 ) ;
#19198 = EDGE_CURVE ( 'NONE', #10799, #13026, #9254, .T. ) ;
#19199 = ORIENTED_EDGE ( 'NONE', *, *, #20180, .F. ) ;
#19200 = DIRECTION ( 'NONE',  ( 0.000000000000000000, 1.000000000000000000, -1.287488025362403787E-15 ) ) ;
#19201 = ORIENTED_EDGE ( 'NONE', *, *, #15487, .T. ) ;
#19202 = CARTESIAN_POINT ( 'NONE',  ( 7.500000000000000000, 4.330127018922190096, -7.422398894150032511 ) ) ;
#19203 = DIRECTION ( 'NONE',  ( 0.000000000000000000, -0.5000000000000009992, -0.8660254037844380415 ) ) ;
#19204 = ORIENTED_EDGE ( 'NONE', *, *, #8549, .T. ) ;
#19205 = VECTOR ( 'NONE', #14248, 1000.000000000000227 ) ;
#19206 = CARTESIAN_POINT ( 'NONE',  ( -280.9952621458756994, 268.8927021017106540, 146.8958543268122128 ) ) ;
#19207 = VECTOR ( 'NONE', #18796, 1000.000000000000000 ) ;
#19208 = ORIENTED_EDGE ( 'NONE', *, *, #23350, .F. ) ;
#19209 = AXIS2_PLACEMENT_3D ( 'NONE', #11712, #568, #9640 ) ;
#19210 = DIRECTION ( 'NONE',  ( 0.000000000000000000, -0.000000000000000000, 1.000000000000000000 ) ) ;
#19211 = DIRECTION ( 'NONE',  ( 0.000000000000000000, 0.000000000000000000, -1.000000000000000000 ) ) ;
#19212 = VECTOR ( 'NONE', #20867, 1000.000000000000000 ) ;
#19213 = CARTESIAN_POINT ( 'NONE',  ( -123.1824219776882785, 83.04955713735502343, 30.00000000000641975 ) ) ;
#19214 = B_SPLINE_CURVE_WITH_KNOTS ( 'NONE', 3,
 ( #1631, #7316, #10862, #14702, #3198 ),
 .UNSPECIFIED., .F., .F.,
 ( 4, 1, 4 ),
 ( 0.000000000000000000, 0.002309401076758505790, 0.004618802153517011580 ),
 .UNSPECIFIED. ) ;
#19215 = DIRECTION ( 'NONE',  ( -1.000000000000000000, -0.000000000000000000, -0.000000000000000000 ) ) ;
#19216 = EDGE_LOOP ( 'NONE', ( #23325, #15176, #12398, #5745, #18108, #9693, #7453, #6652 ) ) ;
#19217 = DIRECTION ( 'NONE',  ( 1.000000000000000000, 0.000000000000000000, 0.000000000000000000 ) ) ;
#19219 = ORIENTED_EDGE ( 'NONE', *, *, #20881, .F. ) ;
#19218 = VERTEX_POINT ( 'NONE', #7972 ) ;
#19220 = VECTOR ( 'NONE', #6588, 1000.000000000000000 ) ;
#19221 = DIRECTION ( 'NONE',  ( 0.000000000000000000, 0.000000000000000000, 1.000000000000000000 ) ) ;
#19222 = EDGE_CURVE ( 'NONE', #12526, #13534, #4817, .T. ) ;
#19223 = EDGE_CURVE ( 'NONE', #10120, #629, #18491, .T. ) ;
#19224 = VECTOR ( 'NONE', #21341, 1000.000000000000114 ) ;
#19225 = CARTESIAN_POINT ( 'NONE',  ( -5.000000000000000888, 5.773502691896258199, -7.063244554130002406 ) ) ;
#19226 = CARTESIAN_POINT ( 'NONE',  ( -146.0000000000000568, -784.4690652294805204, 32.05500000000641592 ) ) ;
#19227 = EDGE_CURVE ( 'NONE', #19560, #13294, #22924, .T. ) ;
#19228 = AXIS2_PLACEMENT_3D ( 'NONE', #4646, #2814, #13854 ) ;
#19229 = AXIS2_PLACEMENT_3D ( 'NONE', #19286, #4327, #11733 ) ;
#19230 = VECTOR ( 'NONE', #11060, 1000.000000000000000 ) ;
#19231 = DIRECTION ( 'NONE',  ( 1.000000000000000000, 0.000000000000000000, 0.000000000000000000 ) ) ;
#19232 = CARTESIAN_POINT ( 'NONE',  ( 50.00000000000000000, 0.000000000000000000, 4.171999999999999709 ) ) ;
#19233 = ORIENTED_EDGE ( 'NONE', *, *, #4871, .T. ) ;
#19234 = CIRCLE ( 'NONE', #11179, 4.250000000000000000 ) ;
#19235 = APPLICATION_CONTEXT ( 'automotive_design' ) ;
#19236 = LINE ( 'NONE', #8621, #22643 ) ;
#19237 = DIRECTION ( 'NONE',  ( 0.000000000000000000, 0.000000000000000000, 1.000000000000000000 ) ) ;
#19238 = CARTESIAN_POINT ( 'NONE',  ( 123.1512869713297960, -1094.121033843497116, 31.25900233431386965 ) ) ;
#19239 = VERTEX_POINT ( 'NONE', #17152 ) ;
#19240 = CARTESIAN_POINT ( 'NONE',  ( -140.0355749532208449, -37.61698748598667663, -2.775557561562891351E-14 ) ) ;
#19241 = VERTEX_POINT ( 'NONE', #15353 ) ;
#19243 = DIRECTION ( 'NONE',  ( 1.000000000000000000, -3.491481338843133355E-15, 0.000000000000000000 ) ) ;
#19242 = VECTOR ( 'NONE', #11186, 1000.000000000000000 ) ;
#19244 = VECTOR ( 'NONE', #20297, 1000.000000000000000 ) ;
#19245 = LINE ( 'NONE', #13514, #21037 ) ;
#19246 = AXIS2_PLACEMENT_3D ( 'NONE', #15515, #6673, #14067 ) ;
#19247 = ORIENTED_EDGE ( 'NONE', *, *, #2339, .T. ) ;
#19248 = CIRCLE ( 'NONE', #3108, 7.500000000000003553 ) ;
#19249 = CARTESIAN_POINT ( 'NONE',  ( 18.83879023463320124, 16.51661848982829284, -145.0000000000000000 ) ) ;
#19250 = ORIENTED_EDGE ( 'NONE', *, *, #13600, .F. ) ;
#19251 = AXIS2_PLACEMENT_3D ( 'NONE', #5486, #1622, #16365 ) ;
#19252 = CARTESIAN_POINT ( 'NONE',  ( 45.00000000000004974, -52.79999999999964899, 107.6500000000002046 ) ) ;
#19253 = CIRCLE ( 'NONE', #11992, 5.560781378645573980 ) ;
#19254 = FACE_OUTER_BOUND ( 'NONE', #12439, .T. ) ;
#19255 = DIRECTION ( 'NONE',  ( 0.000000000000000000, 0.000000000000000000, 1.000000000000000000 ) ) ;
#19256 = DIRECTION ( 'NONE',  ( 1.000000000000000000, 0.000000000000000000, 0.000000000000000000 ) ) ;
#19257 = CARTESIAN_POINT ( 'NONE',  ( 34.99999999999999289, 0.000000000000000000, 2.055000000000000160 ) ) ;
#19258 = DIRECTION ( 'NONE',  ( 0.000000000000000000, 0.000000000000000000, -1.000000000000000000 ) ) ;
#19259 = ORIENTED_EDGE ( 'NONE', *, *, #19759, .F. ) ;
#19260 = CARTESIAN_POINT ( 'NONE',  ( 21.68333333333335844, -89.99999999999998579, 3.000000000000000000 ) ) ;
#19261 = FACE_OUTER_BOUND ( 'NONE', #23455, .T. ) ;
#19262 = ORIENTED_EDGE ( 'NONE', *, *, #18667, .T. ) ;
#19263 = ORIENTED_EDGE ( 'NONE', *, *, #3305, .T. ) ;
#19264 = DIRECTION ( 'NONE',  ( 2.220299922379603824E-16, 1.000000000000000000, 0.000000000000000000 ) ) ;
#19265 = CYLINDRICAL_SURFACE ( 'NONE', #15753, 2.500000000000002220 ) ;
#19267 = CIRCLE ( 'NONE', #5788, 20.00000000000000000 ) ;
#19266 = AXIS2_PLACEMENT_3D ( 'NONE', #13253, #22382, #5844 ) ;
#19268 = STYLED_ITEM ( 'NONE', ( #11910 ), #22822 ) ;
#19269 = AXIS2_PLACEMENT_3D ( 'NONE', #15135, #13339, #20651 ) ;
#19270 = AXIS2_PLACEMENT_3D ( 'NONE', #7603, #14995, #22338 ) ;
#19271 = CARTESIAN_POINT ( 'NONE',  ( -194.7500000000004832, -204.4690652294793836, -29.99999999999322498 ) ) ;
#19272 = CIRCLE ( 'NONE', #3069, 2.500000000000002220 ) ;
#19273 = DIRECTION ( 'NONE',  ( -0.9510565162951557516, 0.3090169943749406234, 0.000000000000000000 ) ) ;
#19274 = LINE ( 'NONE', #23005, #11709 ) ;
#19275 = VECTOR ( 'NONE', #4550, 1000.000000000000000 ) ;
#19276 = CARTESIAN_POINT ( 'NONE',  ( 5.000000000000000000, -2.342598717236900718, 4.057500000000001883 ) ) ;
#19277 = ORIENTED_EDGE ( 'NONE', *, *, #20885, .T. ) ;
#19278 = CARTESIAN_POINT ( 'NONE',  ( -140.0355749532211007, 37.61698748598567477, -90.00000000000000000 ) ) ;
#19279 = LINE ( 'NONE', #15680, #15067 ) ;
#19280 = CYLINDRICAL_SURFACE ( 'NONE', #12550, 7.500000000000007105 ) ;
#19281 = EDGE_LOOP ( 'NONE', ( #11787, #16510, #15800, #1234 ) ) ;
#19282 = FACE_OUTER_BOUND ( 'NONE', #21126, .T. ) ;
#19283 = ITEM_DEFINED_TRANSFORMATION ( 'NONE', 'NONE', #1903,  #11210 ) ;
#19284 = CARTESIAN_POINT ( 'NONE',  ( 37.61698748598715980, -140.0355749532207028, -2.775557561562891351E-14 ) ) ;
#19285 = PRODUCT_DEFINITION_FORMATION_WITH_SPECIFIED_SOURCE ( 'ANY', '', #17885, .NOT_KNOWN. ) ;
#19286 = CARTESIAN_POINT ( 'NONE',  ( -117.3074641843669781, -85.22886158240918064, 90.00000000000000000 ) ) ;
#19287 = VECTOR ( 'NONE', #20481, 1000.000000000000000 ) ;
#19288 = ADVANCED_FACE ( 'NONE', ( #17275, #6163 ), #13443, .T. ) ;
#19289 = CARTESIAN_POINT ( 'NONE',  ( -280.6816199723483578, 272.9663417894423105, 145.1245861693739698 ) ) ;
#19290 = AXIS2_PLACEMENT_3D ( 'NONE', #15461, #19038, #22429 ) ;
#19291 = AXIS2_PLACEMENT_3D ( 'NONE', #7683, #15437, #563 ) ;
#19292 = ORIENTED_EDGE ( 'NONE', *, *, #8357, .F. ) ;
#19293 = EDGE_LOOP ( 'NONE', ( #7510, #10875, #8563, #18502 ) ) ;
#19294 = CARTESIAN_POINT ( 'NONE',  ( 0.000000000000000000, 0.000000000000000000, -90.00000000000000000 ) ) ;
#19295 = CARTESIAN_POINT ( 'NONE',  ( -5.007715329123872641E-16, -8.660254037844399733, -7.422398894150038728 ) ) ;
#19296 = VERTEX_POINT ( 'NONE', #10159 ) ;
#19297 = EDGE_CURVE ( 'NONE', #6984, #9249, #13582, .T. ) ;
#19298 = EDGE_CURVE ( 'NONE', #15625, #14084, #18816, .T. ) ;
#19299 = ORIENTED_EDGE ( 'NONE', *, *, #5227, .F. ) ;
#19300 = CARTESIAN_POINT ( 'NONE',  ( 158.0000000000000284, -500.0000000000000000, 32.64999999999999858 ) ) ;
#19301 = CARTESIAN_POINT ( 'NONE',  ( -280.0000000000000568, 272.9999999999999432, 145.0000000000000284 ) ) ;
#19302 = CARTESIAN_POINT ( 'NONE',  ( 7.497491405671719455, -144.8060344827586334, 90.00000000000000000 ) ) ;
#19303 = ORIENTED_EDGE ( 'NONE', *, *, #16963, .F. ) ;
#19304 = DIRECTION ( 'NONE',  ( 0.000000000000000000, 0.000000000000000000, 1.000000000000000000 ) ) ;
#19305 = EDGE_CURVE ( 'NONE', #9885, #14788, #2529, .T. ) ;
#19306 = VERTEX_POINT ( 'NONE', #2290 ) ;
#19307 = CARTESIAN_POINT ( 'NONE',  ( -4.101948962585905356, -2.368261337751088824, -3.681124513963624167 ) ) ;
#19308 = DIRECTION ( 'NONE',  ( -3.736327486719275871E-16, 1.000000000000000000, 0.000000000000000000 ) ) ;
#19309 = ORIENTED_EDGE ( 'NONE', *, *, #19013, .T. ) ;
#19310 = VERTEX_POINT ( 'NONE', #4222 ) ;
#19311 = CARTESIAN_POINT ( 'NONE',  ( 1.287237434362044075, 3.875615274277557809, -3.430618716626812059 ) ) ;
#19312 = PRODUCT_DEFINITION_SHAPE ( 'NONE', 'NONE',  #23862 ) ;
#19313 = CARTESIAN_POINT ( 'NONE',  ( 4.175648173966055587, -2.207990556236547608, -3.469390959564065291 ) ) ;
#19314 = CYLINDRICAL_SURFACE ( 'NONE', #16316, 2.649999999999971934 ) ;
#19315 = B_SPLINE_CURVE_WITH_KNOTS ( 'NONE', 3,
 ( #1936, #18480, #14757, #9326, #9689, #22090, #17043, #384, #11645, #5815, #11153, #18822, #16680, #2295, #497, #7746 ),
 .UNSPECIFIED., .F., .F.,
 ( 4, 2, 2, 2, 2, 2, 2, 4 ),
 ( 0.000000000000000000, 0.0009361184303672340353, 0.001404177645550768599, 0.001872236860734303489, 0.002340296075917837944, 0.002808355291101372834, 0.003276414506284907290, 0.003744473721468442179 ),
 .UNSPECIFIED. ) ;
#19316 = ORIENTED_EDGE ( 'NONE', *, *, #1215, .F. ) ;
#19317 = FACE_OUTER_BOUND ( 'NONE', #18463, .T. ) ;
#19318 = FILL_AREA_STYLE_COLOUR ( '', #19667 ) ;
#19319 = ORIENTED_EDGE ( 'NONE', *, *, #13231, .T. ) ;
#19320 = ORIENTED_EDGE ( 'NONE', *, *, #6019, .T. ) ;
#19321 = CARTESIAN_POINT ( 'NONE',  ( 8.050072860924167628, -23.72540896942268773, -145.0000000000000000 ) ) ;
#19322 = EDGE_LOOP ( 'NONE', ( #22821, #13365, #5355, #10290, #23536 ) ) ;
#19323 = LINE ( 'NONE', #4964, #6741 ) ;
#19324 = ADVANCED_FACE ( 'NONE', ( #11642, #8109 ), #5911, .F. ) ;
#19325 = FACE_BOUND ( 'NONE', #8465, .T. ) ;
#19326 = EDGE_CURVE ( 'NONE', #9785, #1715, #17038, .T. ) ;
#19327 = ORIENTED_EDGE ( 'NONE', *, *, #7406, .F. ) ;
#19328 = CARTESIAN_POINT ( 'NONE',  ( -280.0000000000000568, 273.0299999999999159, 145.0000000000000284 ) ) ;
#19329 = CARTESIAN_POINT ( 'NONE',  ( 2.500000000000000000, 2.357898499370432166, -2.385244779468109755E-15 ) ) ;
#19330 = ORIENTED_EDGE ( 'NONE', *, *, #16358, .T. ) ;
#19331 = EDGE_CURVE ( 'NONE', #9885, #18604, #718, .T. ) ;
#19332 = CARTESIAN_POINT ( 'NONE',  ( -79.99999999999995737, -59.79999999999918714, 250.0000000000000000 ) ) ;
#19333 = DIRECTION ( 'NONE',  ( -3.700743415417187942E-15, 1.000000000000000000, 0.000000000000000000 ) ) ;
#19334 = EDGE_CURVE ( 'NONE', #2037, #14427, #4079, .T. ) ;
#19335 =( NAMED_UNIT ( * ) PLANE_ANGLE_UNIT ( ) SI_UNIT ( $, .RADIAN. ) );
#19336 = CARTESIAN_POINT ( 'NONE',  ( -107.6499999999999631, -29.99999999999998579, 3.000000000000000000 ) ) ;
#19337 = ORIENTED_EDGE ( 'NONE', *, *, #15885, .T. ) ;
#19338 = CARTESIAN_POINT ( 'NONE',  ( 2.500000000000000000, 1.178949249685213863, -2.042000000000001148 ) ) ;
#19339 = SURFACE_STYLE_FILL_AREA ( #5102 ) ;
#19341 = VERTEX_POINT ( 'NONE', #17759 ) ;
#19340 = ORIENTED_EDGE ( 'NONE', *, *, #1321, .T. ) ;
#19342 = DIRECTION ( 'NONE',  ( 0.000000000000000000, 0.000000000000000000, 1.000000000000000000 ) ) ;
#19343 = CARTESIAN_POINT ( 'NONE',  ( 7.922798488042200660, -4.627419312545550056, -8.057411459260041653 ) ) ;
#19344 = DIRECTION ( 'NONE',  ( 1.000000000000000000, -7.709882115452475701E-17, 0.000000000000000000 ) ) ;
#19345 = DIRECTION ( 'NONE',  ( 1.000000000000000000, 0.000000000000000000, 0.000000000000000000 ) ) ;
#19346 = CARTESIAN_POINT ( 'NONE',  ( 7.500000000000000000, 4.330127018922190096, -10.00000000000000000 ) ) ;
#19347 = CARTESIAN_POINT ( 'NONE',  ( -2.999999999999995559, 0.000000000000000000, 0.000000000000000000 ) ) ;
#19348 = EDGE_CURVE ( 'NONE', #14422, #19892, #15947, .T. ) ;
#19349 = ORIENTED_EDGE ( 'NONE', *, *, #3708, .T. ) ;
#19350 = CARTESIAN_POINT ( 'NONE',  ( -37.30746418436748968, 137.9031948627972781, 90.00000000000000000 ) ) ;
#19351 = ADVANCED_BREP_SHAPE_REPRESENTATION ( '', ( #20017, #11210 ), #16580 ) ;
#19352 = DIRECTION ( 'NONE',  ( 0.000000000000000000, 1.110223024625156540E-16, -1.000000000000000000 ) ) ;
#19353 = DIRECTION ( 'NONE',  ( 0.000000000000000000, 0.000000000000000000, -1.000000000000000000 ) ) ;
#19354 = CONTEXT_DEPENDENT_SHAPE_REPRESENTATION ( #17875, #17790 ) ;
#19355 = ORIENTED_EDGE ( 'NONE', *, *, #23742, .T. ) ;
#19356 = AXIS2_PLACEMENT_3D ( 'NONE', #17370, #2495, #18782 ) ;
#19357 = CARTESIAN_POINT ( 'NONE',  ( 45.00000000000002132, -56.79999999999932925, 197.6500000000002046 ) ) ;
#19358 = ORIENTED_EDGE ( 'NONE', *, *, #19738, .F. ) ;
#19359 = DIRECTION ( 'NONE',  ( 0.000000000000000000, 0.000000000000000000, 1.000000000000000000 ) ) ;
#19360 = LINE ( 'NONE', #21663, #8725 ) ;
#19361 = ADVANCED_FACE ( 'NONE', ( #15840 ), #1315, .F. ) ;
#19362 = ORIENTED_EDGE ( 'NONE', *, *, #8706, .T. ) ;
#19363 = EDGE_CURVE ( 'NONE', #21483, #9371, #21214, .T. ) ;
#19364 = CARTESIAN_POINT ( 'NONE',  ( -18.83866108947328755, 16.51660830833442262, -145.0000000000000000 ) ) ;
#19365 = ORIENTED_EDGE ( 'NONE', *, *, #11723, .F. ) ;
#19366 = DIRECTION ( 'NONE',  ( 1.000000000000000000, 0.000000000000000000, 0.000000000000000000 ) ) ;
#19367 = CARTESIAN_POINT ( 'NONE',  ( 85.22886158240706322, 117.3074641843685129, 90.00000000000000000 ) ) ;
#19368 = DIRECTION ( 'NONE',  ( 0.000000000000000000, 1.000000000000000000, -1.224646799147353207E-16 ) ) ;
#19369 = CARTESIAN_POINT ( 'NONE',  ( 0.000000000000000000, 0.000000000000000000, 90.00000000000000000 ) ) ;
#19370 = DIRECTION ( 'NONE',  ( 0.000000000000000000, -1.000000000000000000, 1.295896757998781966E-15 ) ) ;
#19371 = ORIENTED_EDGE ( 'NONE', *, *, #15942, .F. ) ;
#19372 = DIRECTION ( 'NONE',  ( -0.000000000000000000, 0.000000000000000000, -1.000000000000000000 ) ) ;
#19373 = DIRECTION ( 'NONE',  ( -1.350636282998972974E-14, 0.000000000000000000, -1.000000000000000000 ) ) ;
#19374 = ORIENTED_EDGE ( 'NONE', *, *, #7934, .T. ) ;
#19375 = AXIS2_PLACEMENT_3D ( 'NONE', #7007, #1, #9174 ) ;
#19376 = ORIENTED_EDGE ( 'NONE', *, *, #16972, .F. ) ;
#19377 = CARTESIAN_POINT ( 'NONE',  ( 281.4928932188134354, -132.2000000000000455, -152.4000000000013131 ) ) ;
#19378 = CARTESIAN_POINT ( 'NONE',  ( 45.00000000000002132, -56.79999999999934346, 192.3500000000002501 ) ) ;
#19379 = CARTESIAN_POINT ( 'NONE',  ( -31.74999999999995737, 0.000000000000000000, 0.000000000000000000 ) ) ;
#19380 = CARTESIAN_POINT ( 'NONE',  ( 131.9719027401098401, 81.29225469460354248, 28.11255663403418126 ) ) ;
#19381 = FACE_OUTER_BOUND ( 'NONE', #23578, .T. ) ;
#19382 = PLANE ( 'NONE',  #1522 ) ;
#19383 = EDGE_LOOP ( 'NONE', ( #17983, #6467, #21995, #7019 ) ) ;
#19384 = LINE ( 'NONE', #19633, #10245 ) ;
#19385 = DIRECTION ( 'NONE',  ( 0.000000000000000000, 0.000000000000000000, -1.000000000000000000 ) ) ;
#19386 = EDGE_CURVE ( 'NONE', #7507, #16244, #23175, .T. ) ;
#19387 = CARTESIAN_POINT ( 'NONE',  ( -20.63749999999999574, 0.000000000000000000, -23.50000000000000000 ) ) ;
#19388 = ORIENTED_EDGE ( 'NONE', *, *, #12252, .T. ) ;
#19389 = DIRECTION ( 'NONE',  ( 0.000000000000000000, 0.000000000000000000, -1.000000000000000000 ) ) ;
#19390 = CIRCLE ( 'NONE', #9002, 7.500000000000001776 ) ;
#19391 = EDGE_CURVE ( 'NONE', #5386, #4309, #15710, .T. ) ;
#19392 = FACE_OUTER_BOUND ( 'NONE', #10623, .T. ) ;
#19393 = CARTESIAN_POINT ( 'NONE',  ( -24.19924082430739887, -1006.487720809339407, -145.0000000000000568 ) ) ;
#19394 = LINE ( 'NONE', #20735, #11573 ) ;
#19395 = CARTESIAN_POINT ( 'NONE',  ( -3.093157300003891663, -6.874418838041293611, -6.051203375184721622E-15 ) ) ;
#19396 = ORIENTED_EDGE ( 'NONE', *, *, #19963, .T. ) ;
#19397 = ORIENTED_EDGE ( 'NONE', *, *, #23771, .F. ) ;
#19398 = CARTESIAN_POINT ( 'NONE',  ( -280.9942590117597661, 268.9045205713627524, -146.9080393212555862 ) ) ;
#19399 = CARTESIAN_POINT ( 'NONE',  ( 0.000000000000000000, -1.178949249685213863, 2.042000000000001148 ) ) ;
#19400 = ORIENTED_EDGE ( 'NONE', *, *, #22250, .T. ) ;
#19401 = VECTOR ( 'NONE', #10964, 1000.000000000000000 ) ;
#19402 = VECTOR ( 'NONE', #4123, 1000.000000000000000 ) ;
#19403 = B_SPLINE_CURVE_WITH_KNOTS ( 'NONE', 3,
 ( #11068, #6953, #18388, #1727, #9001, #23486 ),
 .UNSPECIFIED., .F., .F.,
 ( 4, 2, 4 ),
 ( 0.004615310220740742597, 0.006918661718823353700, 0.009222013216905964803 ),
 .UNSPECIFIED. ) ;
#19404 = EDGE_LOOP ( 'NONE', ( #6966, #17631, #3295 ) ) ;
#19405 = DIRECTION ( 'NONE',  ( 0.000000000000000000, 0.000000000000000000, -1.000000000000000000 ) ) ;
#19406 = CARTESIAN_POINT ( 'NONE',  ( -127.7150463208625553, 87.82877071840113103, 32.48389983298811501 ) ) ;
#19407 = ORIENTED_EDGE ( 'NONE', *, *, #16312, .F. ) ;
#19408 = CARTESIAN_POINT ( 'NONE',  ( -135.1739945062392394, -1075.849084086415360, -27.81095155082704196 ) ) ;
#19409 = EDGE_CURVE ( 'NONE', #1461, #23519, #14390, .T. ) ;
#19410 = EDGE_LOOP ( 'NONE', ( #13533, #23669, #15964, #12835 ) ) ;
#19411 = EDGE_CURVE ( 'NONE', #17109, #6763, #3465, .T. ) ;
#19412 = DIRECTION ( 'NONE',  ( 1.000000000000000000, 0.000000000000000000, 0.000000000000000000 ) ) ;
#19413 = DIRECTION ( 'NONE',  ( -1.000000000000000000, 0.000000000000000000, -0.000000000000000000 ) ) ;
#19414 = ORIENTED_EDGE ( 'NONE', *, *, #15523, .T. ) ;
#19415 = VERTEX_POINT ( 'NONE', #12361 ) ;
#19416 = CARTESIAN_POINT ( 'NONE',  ( 134.0852850658434079, 77.75691219176877667, -29.34813586885359271 ) ) ;
#19417 = AXIS2_PLACEMENT_3D ( 'NONE', #14605, #1312, #10645 ) ;
#19418 = EDGE_CURVE ( 'NONE', #21068, #16414, #7305, .T. ) ;
#19419 = CARTESIAN_POINT ( 'NONE',  ( -280.8082263737021549, 271.2379565153278804, -148.9159870726003874 ) ) ;
#19420 = AXIS2_PLACEMENT_3D ( 'NONE', #9624, #13165, #12915 ) ;
#19421 = LINE ( 'NONE', #7771, #12325 ) ;
#19422 = DIRECTION ( 'NONE',  ( 1.000000000000000000, 0.000000000000000000, 0.000000000000000000 ) ) ;
#19423 = ORIENTED_EDGE ( 'NONE', *, *, #14325, .F. ) ;
#19424 = CARTESIAN_POINT ( 'NONE',  ( 281.4928932188133217, -132.2000000000000455, 177.2000000000014097 ) ) ;
#19425 = EDGE_CURVE ( 'NONE', #4511, #8574, #21727, .T. ) ;
#19426 = EDGE_LOOP ( 'NONE', ( #903, #13122, #5683, #2879 ) ) ;
#19427 = ORIENTED_EDGE ( 'NONE', *, *, #9319, .F. ) ;
#19428 = COLOUR_RGB ( '',0.8941176470588234615, 0.8941176470588234615, 0.8941176470588234615 ) ;
#19429 = CARTESIAN_POINT ( 'NONE',  ( 19.87455415541893444, -15.25449798594880058, -145.0000000000000000 ) ) ;
#19430 = AXIS2_PLACEMENT_3D ( 'NONE', #19367, #1009, #13748 ) ;
#19431 = VERTEX_POINT ( 'NONE', #3705 ) ;
#19432 = LINE ( 'NONE', #12499, #3304 ) ;
#19433 = CIRCLE ( 'NONE', #14456, 2.649999999999999467 ) ;
#19434 = CARTESIAN_POINT ( 'NONE',  ( -31.74999999999995737, 0.000000000000000000, 4.250000000000000000 ) ) ;
#19435 = ORIENTED_EDGE ( 'NONE', *, *, #4353, .T. ) ;
#19436 = CARTESIAN_POINT ( 'NONE',  ( -281.4928932188135491, 267.7999999999999545, 147.1696999999999775 ) ) ;
#19437 = DIRECTION ( 'NONE',  ( 0.6964005597823107463, -0.7176533009294141507, 6.982962677686266711E-15 ) ) ;
#19438 = ORIENTED_EDGE ( 'NONE', *, *, #13208, .F. ) ;
#19439 = ADVANCED_FACE ( 'NONE', ( #7218 ), #22303, .F. ) ;
#19440 = CARTESIAN_POINT ( 'NONE',  ( 171.6502151485116485, 95.33502053007514121, -29.99999999999322498 ) ) ;
#19441 = EDGE_CURVE ( 'NONE', #5160, #7573, #16576, .T. ) ;
#19442 = B_SPLINE_CURVE_WITH_KNOTS ( 'NONE', 3,
 ( #17800, #1361, #8261, #23217, #10572, #6802, #17910, #21526 ),
 .UNSPECIFIED., .F., .F.,
 ( 4, 2, 2, 4 ),
 ( 0.006061689441712453386, 0.007174127271521678166, 0.008286565101330902947, 0.01051144076094935251 ),
 .UNSPECIFIED. ) ;
#19443 = AXIS2_PLACEMENT_3D ( 'NONE', #20327, #5854, #5613 ) ;
#19444 = DIRECTION ( 'NONE',  ( 0.000000000000000000, 0.000000000000000000, 1.000000000000000000 ) ) ;
#19445 = ORIENTED_EDGE ( 'NONE', *, *, #19048, .F. ) ;
#19446 = FACE_OUTER_BOUND ( 'NONE', #984, .T. ) ;
#19447 = EDGE_CURVE ( 'NONE', #7773, #4083, #108, .T. ) ;
#19448 = VECTOR ( 'NONE', #16084, 1000.000000000000000 ) ;
#19449 = ADVANCED_FACE ( 'NONE', ( #11005 ), #15443, .T. ) ;
#19451 = ORIENTED_EDGE ( 'NONE', *, *, #3633, .F. ) ;
#19450 = VERTEX_POINT ( 'NONE', #20141 ) ;
#19452 = CIRCLE ( 'NONE', #7894, 2.649999999999971934 ) ;
#19453 = DIRECTION ( 'NONE',  ( 1.000000000000000000, 0.000000000000000000, 6.123233995736766036E-17 ) ) ;
#19454 = PLANE ( 'NONE',  #21978 ) ;
#19455 = DIRECTION ( 'NONE',  ( -1.000000000000000000, 0.000000000000000000, 0.000000000000000000 ) ) ;
#19456 = DIRECTION ( 'NONE',  ( -1.000000000000000000, 0.000000000000000000, -0.000000000000000000 ) ) ;
#19457 = DIRECTION ( 'NONE',  ( -1.000000000000000000, -0.000000000000000000, -0.000000000000000000 ) ) ;
#19458 = CARTESIAN_POINT ( 'NONE',  ( 89.00000000000000000, -74.99999999999998579, 3.000000000000000000 ) ) ;
#19459 = EDGE_CURVE ( 'NONE', #18832, #5216, #20368, .T. ) ;
#19460 = CONICAL_SURFACE ( 'NONE', #3283, 2.055000000000000160, 0.7853981633974639331 ) ;
#19461 = ORIENTED_EDGE ( 'NONE', *, *, #5471, .T. ) ;
#19462 = SHAPE_REPRESENTATION ( 'motor mounting flange', ( #11210 ), #6181 ) ;
#19463 = DIRECTION ( 'NONE',  ( 0.000000000000000000, 0.4999999999999991118, -0.8660254037844391517 ) ) ;
#19464 = VERTEX_POINT ( 'NONE', #21954 ) ;
#19465 = LINE ( 'NONE', #2921, #21001 ) ;
#19466 = DIRECTION ( 'NONE',  ( 0.000000000000000000, -1.000000000000000000, 0.000000000000000000 ) ) ;
#19467 = CONTEXT_DEPENDENT_SHAPE_REPRESENTATION ( #16328, #982 ) ;
#19468 = ORIENTED_EDGE ( 'NONE', *, *, #6868, .T. ) ;
#19469 = PRESENTATION_LAYER_ASSIGNMENT (  '', '', ( #15268 ) ) ;
#19470 = CYLINDRICAL_SURFACE ( 'NONE', #16765, 2.649999999999985700 ) ;
#19471 = ORIENTED_EDGE ( 'NONE', *, *, #15096, .F. ) ;
#19472 = PLANE ( 'NONE',  #8473 ) ;
#19473 = DIRECTION ( 'NONE',  ( 0.000000000000000000, 0.000000000000000000, 1.000000000000000000 ) ) ;
#19474 = ORIENTED_EDGE ( 'NONE', *, *, #10406, .T. ) ;
#19475 =( NAMED_UNIT ( * ) SI_UNIT ( $, .STERADIAN. ) SOLID_ANGLE_UNIT ( ) );
#19476 = LINE ( 'NONE', #19252, #3035 ) ;
#19477 = CARTESIAN_POINT ( 'NONE',  ( 5.000000000000000000, -2.342598717236910488, -4.057499999999997442 ) ) ;
#19478 = CARTESIAN_POINT ( 'NONE',  ( -129.6400180686271142, -1072.557589128678273, -29.99999999999356248 ) ) ;
#19479 = EDGE_CURVE ( 'NONE', #5970, #2346, #7821, .T. ) ;
#19480 = CARTESIAN_POINT ( 'NONE',  ( 281.3429506979391590, 269.5484459290825043, 145.6225751257468062 ) ) ;
#19481 = AXIS2_PLACEMENT_3D ( 'NONE', #17373, #1170, #814 ) ;
#19482 = CARTESIAN_POINT ( 'NONE',  ( -146.0000000000000853, -494.4690652294807478, 30.00000000000641620 ) ) ;
#19483 = EDGE_CURVE ( 'NONE', #15690, #885, #22690, .T. ) ;
#19484 = CARTESIAN_POINT ( 'NONE',  ( -31.74999999999995737, 0.000000000000000000, 0.000000000000000000 ) ) ;
#19485 = ADVANCED_FACE ( 'NONE', ( #20253 ), #11252, .T. ) ;
#19486 = ORIENTED_EDGE ( 'NONE', *, *, #22375, .T. ) ;
#19487 = AXIS2_PLACEMENT_3D ( 'NONE', #9066, #14, #16780 ) ;
#19488 = EDGE_CURVE ( 'NONE', #8023, #13119, #4967, .T. ) ;
#19489 = FACE_OUTER_BOUND ( 'NONE', #15824, .T. ) ;
#19490 = CARTESIAN_POINT ( 'NONE',  ( 110.0000000000000000, 95.00000000000000000, 0.000000000000000000 ) ) ;
#19491 = EDGE_LOOP ( 'NONE', ( #1324, #9565 ) ) ;
#19492 = AXIS2_PLACEMENT_3D ( 'NONE', #8167, #22507, #6334 ) ;
#19493 = ORIENTED_EDGE ( 'NONE', *, *, #16399, .F. ) ;
#19494 = DIRECTION ( 'NONE',  ( 8.144298233840332611E-17, 3.483493295888648978E-15, 1.000000000000000000 ) ) ;
#19495 = CARTESIAN_POINT ( 'NONE',  ( -4.000000000000000000, -2.309401076758512694, -3.433295621305382461 ) ) ;
#19496 = ADVANCED_FACE ( 'NONE', ( #9406 ), #15768, .T. ) ;
#19497 = ADVANCED_FACE ( 'NONE', ( #9170 ), #21350, .F. ) ;
#19499 = LINE ( 'NONE', #8187, #5973 ) ;
#19498 = PRODUCT_DEFINITION_SHAPE ( 'NONE', 'NONE',  #23881 ) ;
#19500 = B_SPLINE_CURVE_WITH_KNOTS ( 'NONE', 3,
 ( #15631, #2703, #1237, #6315, #17538, #19225, #6794, #23329, #19573 ),
 .UNSPECIFIED., .F., .F.,
 ( 4, 2, 1, 2, 4 ),
 ( 0.000000000000000000, 0.002165063509461098365, 0.004330127018922195863, 0.006495190528383293360, 0.008660254037844389990 ),
 .UNSPECIFIED. ) ;
#19501 = CONICAL_SURFACE ( 'NONE', #16068, 2.055000000000001492, 0.7853981633974633780 ) ;
#19502 = CARTESIAN_POINT ( 'NONE',  ( 132.1836189744865919, 80.94757571328977974, 27.82811892742372351 ) ) ;
#19503 = CARTESIAN_POINT ( 'NONE',  ( -35.00000000000000000, 0.000000000000000000, 100.0000000000000000 ) ) ;
#19504 = CARTESIAN_POINT ( 'NONE',  ( 5.000000000000002665, 3.306546357697854226E-16, 2.700000000000000622 ) ) ;
#19505 = VERTEX_POINT ( 'NONE', #20982 ) ;
#19506 = DIRECTION ( 'NONE',  ( 0.000000000000000000, 0.000000000000000000, 1.000000000000000000 ) ) ;
#19507 = CARTESIAN_POINT ( 'NONE',  ( 5.000000000000000000, 2.342598717236902939, -4.057500000000001883 ) ) ;
#19508 = DIRECTION ( 'NONE',  ( 0.7071067811865320296, 8.659560562355062281E-17, 0.7071067811865631159 ) ) ;
#19509 = ORIENTED_EDGE ( 'NONE', *, *, #6318, .F. ) ;
#19510 = SURFACE_STYLE_FILL_AREA ( #4793 ) ;
#19511 = CYLINDRICAL_SURFACE ( 'NONE', #11120, 145.0000000000000284 ) ;
#19512 = LINE ( 'NONE', #2964, #6960 ) ;
#19513 = DIRECTION ( 'NONE',  ( -0.000000000000000000, 1.000000000000000000, -0.000000000000000000 ) ) ;
#19514 = DIRECTION ( 'NONE',  ( 0.000000000000000000, 0.7071067811865489050, 0.7071067811865462405 ) ) ;
#19515 = DIRECTION ( 'NONE',  ( 1.000000000000000000, 0.000000000000000000, 0.000000000000000000 ) ) ;
#19516 = CARTESIAN_POINT ( 'NONE',  ( -85.22886158240879695, 117.3074641843673049, -90.00000000000000000 ) ) ;
#19517 = ORIENTED_EDGE ( 'NONE', *, *, #20234, .T. ) ;
#19518 = ORIENTED_EDGE ( 'NONE', *, *, #12743, .F. ) ;
#19519 = CARTESIAN_POINT ( 'NONE',  ( -281.0571734979477014, 268.7755403010746136, -146.9771302778488007 ) ) ;
#19520 = CIRCLE ( 'NONE', #22999, 5.000000000000002665 ) ;
#19521 = DIRECTION ( 'NONE',  ( -1.000000000000000000, 0.000000000000000000, 0.000000000000000000 ) ) ;
#19522 = ORIENTED_EDGE ( 'NONE', *, *, #22580, .F. ) ;
#19523 = DIRECTION ( 'NONE',  ( -0.000000000000000000, -0.000000000000000000, -1.000000000000000000 ) ) ;
#19524 = CARTESIAN_POINT ( 'NONE',  ( -20.00000000000000000, 2.449293598294706513E-15, 100.0000000000000000 ) ) ;
#19525 = EDGE_CURVE ( 'NONE', #10936, #3608, #6134, .T. ) ;
#19526 = ADVANCED_FACE ( 'NONE', ( #17376 ), #18446, .T. ) ;
#19527 = VERTEX_POINT ( 'NONE', #344 ) ;
#19528 = CARTESIAN_POINT ( 'NONE',  ( -69.99999999999997158, -87.33333333333338544, 124.9999999999999858 ) ) ;
#19529 = CARTESIAN_POINT ( 'NONE',  ( 4.336808689942017736E-16, 8.660254037844390851, -1.000000000000000888 ) ) ;
#19530 = VERTEX_POINT ( 'NONE', #9893 ) ;
#19531 = DIRECTION ( 'NONE',  ( 0.000000000000000000, -1.000000000000000000, 0.000000000000000000 ) ) ;
#19532 = VECTOR ( 'NONE', #17993, 1000.000000000000000 ) ;
#19533 = ORIENTED_EDGE ( 'NONE', *, *, #18895, .T. ) ;
#19534 = CIRCLE ( 'NONE', #18377, 2.055000000000001492 ) ;
#19535 = CARTESIAN_POINT ( 'NONE',  ( 0.000000000000000000, 0.000000000000000000, 90.00000000000000000 ) ) ;
#19536 = DIRECTION ( 'NONE',  ( -0.000000000000000000, -0.000000000000000000, 1.000000000000000000 ) ) ;
#19537 = ORIENTED_EDGE ( 'NONE', *, *, #14771, .T. ) ;
#19538 = ORIENTED_EDGE ( 'NONE', *, *, #22169, .T. ) ;
#19539 = CARTESIAN_POINT ( 'NONE',  ( 133.9966253006742534, 77.90961723643309256, -31.11320915316591496 ) ) ;
#19540 = APPLICATION_PROTOCOL_DEFINITION ( 'draft international standard', 'automotive_design', 1998, #21391 ) ;
#19541 = FACE_OUTER_BOUND ( 'NONE', #7616, .T. ) ;
#19542 = LINE ( 'NONE', #15844, #22677 ) ;
#19543 = LINE ( 'NONE', #3138, #505 ) ;
#19544 = ORIENTED_EDGE ( 'NONE', *, *, #14939, .F. ) ;
#19545 = LINE ( 'NONE', #3004, #5292 ) ;
#19546 = CIRCLE ( 'NONE', #7605, 20.00000000000000000 ) ;
#19547 = APPLICATION_CONTEXT ( 'automotive_design' ) ;
#19548 = EDGE_LOOP ( 'NONE', ( #9530, #13264, #7432, #23574 ) ) ;
#19549 = CIRCLE ( 'NONE', #11903, 2.649999999999985700 ) ;
#19550 = AXIS2_PLACEMENT_3D ( 'NONE', #10616, #17838, #12208 ) ;
#19551 = ORIENTED_EDGE ( 'NONE', *, *, #11141, .F. ) ;
#19552 = FACE_OUTER_BOUND ( 'NONE', #14028, .T. ) ;
#19553 = ORIENTED_EDGE ( 'NONE', *, *, #17571, .T. ) ;
#19554 = CARTESIAN_POINT ( 'NONE',  ( -155.0000000000000284, -494.4690652294799520, -29.99999999999350564 ) ) ;
#19555 = CARTESIAN_POINT ( 'NONE',  ( 0.000000000000000000, 0.000000000000000000, 0.000000000000000000 ) ) ;
#19556 = ORIENTED_EDGE ( 'NONE', *, *, #8453, .T. ) ;
#19557 = LINE ( 'NONE', #20137, #667 ) ;
#19558 = CARTESIAN_POINT ( 'NONE',  ( 100.0000000000000000, -1400.000000000000000, 124.9999999999998295 ) ) ;
#19559 = AXIS2_PLACEMENT_3D ( 'NONE', #22642, #8397, #2831 ) ;
#19560 = VERTEX_POINT ( 'NONE', #20732 ) ;
#19561 = CARTESIAN_POINT ( 'NONE',  ( -0.3208286057739654917, 4.433571671609680465, -0.3503314178412548774 ) ) ;
#19562 = AXIS2_PLACEMENT_3D ( 'NONE', #3990, #17175, #7994 ) ;
#19563 = FACE_BOUND ( 'NONE', #23082, .T. ) ;
#19564 = CARTESIAN_POINT ( 'NONE',  ( -45.00000000000000000, 269.9999999999999432, -5.249999999999973355 ) ) ;
#19565 = AXIS2_PLACEMENT_3D ( 'NONE', #20419, #3880, #5825 ) ;
#19566 = LINE ( 'NONE', #23439, #5747 ) ;
#19567 = ORIENTED_EDGE ( 'NONE', *, *, #8047, .T. ) ;
#19568 = LINE ( 'NONE', #4736, #16933 ) ;
#19569 = PRESENTATION_STYLE_ASSIGNMENT (( #8730 ) ) ;
#19571 = ORIENTED_EDGE ( 'NONE', *, *, #14030, .T. ) ;
#19570 = ORIENTED_EDGE ( 'NONE', *, *, #20391, .F. ) ;
#19572 = CARTESIAN_POINT ( 'NONE',  ( 0.000000000000000000, 0.000000000000000000, -142.0000000000000568 ) ) ;
#19573 = CARTESIAN_POINT ( 'NONE',  ( -7.500000000000000000, 4.330127018922191873, -7.422398894150032511 ) ) ;
#19574 = CARTESIAN_POINT ( 'NONE',  ( 4.000000000000000000, 0.3987449864460005378, -0.01220643443059817035 ) ) ;
#19575 = AXIS2_PLACEMENT_3D ( 'NONE', #1726, #10952, #5483 ) ;
#19576 = LINE ( 'NONE', #6434, #3475 ) ;
#19577 = CARTESIAN_POINT ( 'NONE',  ( 2.500000000000000000, -1.178949249685218748, -2.041999999999998039 ) ) ;
#19578 = ADVANCED_FACE ( 'NONE', ( #11848 ), #16879, .F. ) ;
#19579 = DIRECTION ( 'NONE',  ( 0.000000000000000000, 0.000000000000000000, -1.000000000000000000 ) ) ;
#19580 = CIRCLE ( 'NONE', #22675, 2.649999999999971934 ) ;
#19581 = VECTOR ( 'NONE', #6962, 1000.000000000000000 ) ;
#19582 = ORIENTED_EDGE ( 'NONE', *, *, #19386, .F. ) ;
#19583 = EDGE_CURVE ( 'NONE', #15272, #12933, #7948, .T. ) ;
#19584 = EDGE_CURVE ( 'NONE', #9294, #20797, #13867, .T. ) ;
#19585 = CIRCLE ( 'NONE', #15380, 2.499999999999998668 ) ;
#19586 = CARTESIAN_POINT ( 'NONE',  ( 2.500000000000000000, -2.357898499370431722, 2.818925648462311528E-15 ) ) ;
#19587 = CIRCLE ( 'NONE', #13097, 145.0000000000000284 ) ;
#19588 = EDGE_LOOP ( 'NONE', ( #1730, #8971, #21482, #17976, #23429 ) ) ;
#19589 = CARTESIAN_POINT ( 'NONE',  ( 7.894787914004607998, 1.243647571710251278E-13, -7.591390474663425536 ) ) ;
#19590 = FACE_OUTER_BOUND ( 'NONE', #21817, .T. ) ;
#19591 = ADVANCED_FACE ( 'NONE', ( #15099 ), #1858, .T. ) ;
#19592 = ITEM_DEFINED_TRANSFORMATION ( 'NONE', 'NONE', #6156,  #11210 ) ;
#19593 = EDGE_LOOP ( 'NONE', ( #11402, #13310 ) ) ;
#19594 = FACE_OUTER_BOUND ( 'NONE', #4980, .T. ) ;
#19595 = ORIENTED_EDGE ( 'NONE', *, *, #13701, .T. ) ;
#19596 = DIRECTION ( 'NONE',  ( 0.000000000000000000, 0.8660254037844380415, -0.5000000000000011102 ) ) ;
#19597 = DIRECTION ( 'NONE',  ( -0.000000000000000000, 1.000000000000000000, -0.000000000000000000 ) ) ;
#19598 = EDGE_LOOP ( 'NONE', ( #13944, #21694, #2581, #16659 ) ) ;
#19599 = DIRECTION ( 'NONE',  ( -0.7071067811865416886, 9.961996129952529179E-15, -0.7071067811865532349 ) ) ;
#19600 = PLANE ( 'NONE',  #1111 ) ;
#19601 = CARTESIAN_POINT ( 'NONE',  ( -7.914984360234579519, 3.818534719232089980, -7.907701344400639876 ) ) ;
#19602 = DIRECTION ( 'NONE',  ( 0.000000000000000000, 0.000000000000000000, -1.000000000000000000 ) ) ;
#19603 = AXIS2_PLACEMENT_3D ( 'NONE', #4887, #3180, #6458 ) ;
#19604 = DIRECTION ( 'NONE',  ( -0.6663528160695909586, -0.2365880903936287138, 0.7071067811865631159 ) ) ;
#19605 = DIRECTION ( 'NONE',  ( 0.000000000000000000, -0.5000000000000012212, -0.8660254037844380415 ) ) ;
#19606 = AXIS2_PLACEMENT_3D ( 'NONE', #22277, #22156, #16497 ) ;
#19607 = CARTESIAN_POINT ( 'NONE',  ( -122.8605704798723082, 82.74225173005861222, 30.00000000000641620 ) ) ;
#19608 = VECTOR ( 'NONE', #12143, 1000.000000000000000 ) ;
#19609 = ORIENTED_EDGE ( 'NONE', *, *, #12705, .T. ) ;
#19610 = DIRECTION ( 'NONE',  ( -0.000000000000000000, -0.000000000000000000, 1.000000000000000000 ) ) ;
#19611 = CARTESIAN_POINT ( 'NONE',  ( -4.000000000000000000, -0.8382240730041925492, -3.220610619767135141 ) ) ;
#19612 = CIRCLE ( 'NONE', #1551, 4.250000000000000000 ) ;
#19613 = ORIENTED_EDGE ( 'NONE', *, *, #431, .T. ) ;
#19614 = ORIENTED_EDGE ( 'NONE', *, *, #5291, .F. ) ;
#19615 = CARTESIAN_POINT ( 'NONE',  ( -288.2000000000010687, -19.99999999999898392, 102.3500000000000227 ) ) ;
#19616 = LINE ( 'NONE', #8293, #709 ) ;
#19617 = CARTESIAN_POINT ( 'NONE',  ( 5.000000000000000000, -2.342598717236900718, 4.057500000000001883 ) ) ;
#19618 = ADVANCED_FACE ( 'NONE', ( #818, #4194 ), #11727, .T. ) ;
#19619 = AXIS2_PLACEMENT_3D ( 'NONE', #2221, #13637, #22398 ) ;
#19621 = CONICAL_SURFACE ( 'NONE', #6517, 4.174999999999999822, 0.9599310885968795892 ) ;
#19620 = MECHANICAL_DESIGN_GEOMETRIC_PRESENTATION_REPRESENTATION (  '', ( #16550 ), #10806 ) ;
#19622 = CARTESIAN_POINT ( 'NONE',  ( 131.5154891841469862, 82.02850787876555216, 29.67150201188731629 ) ) ;
#19623 = VECTOR ( 'NONE', #20114, 1000.000000000000000 ) ;
#19624 = CARTESIAN_POINT ( 'NONE',  ( 145.0000000000000284, -500.0000000000000000, -29.99999999999997158 ) ) ;
#19625 = EDGE_CURVE ( 'NONE', #1524, #11269, #2255, .T. ) ;
#19626 = CIRCLE ( 'NONE', #2287, 2.649999999999971934 ) ;
#19627 = EDGE_LOOP ( 'NONE', ( #3173, #699 ) ) ;
#19628 = AXIS2_PLACEMENT_3D ( 'NONE', #6577, #23461, #19353 ) ;
#19629 = VECTOR ( 'NONE', #20407, 1000.000000000000000 ) ;
#19630 = DIRECTION ( 'NONE',  ( 1.000000000000000000, -0.000000000000000000, 6.982962677686266711E-15 ) ) ;
#19631 = EDGE_CURVE ( 'NONE', #3415, #840, #9658, .T. ) ;
#19632 = ORIENTED_EDGE ( 'NONE', *, *, #21867, .F. ) ;
#19633 = CARTESIAN_POINT ( 'NONE',  ( 110.0000000000000000, 95.00000000000000000, 3.000000000000000000 ) ) ;
#19634 = LINE ( 'NONE', #1171, #6131 ) ;
#19635 = LINE ( 'NONE', #5392, #17130 ) ;
#19636 = ORIENTED_EDGE ( 'NONE', *, *, #8151, .F. ) ;
#19637 = CARTESIAN_POINT ( 'NONE',  ( -20.00000000000000000, 2.449293598294706513E-15, -138.9999999999999716 ) ) ;
#19638 = EDGE_CURVE ( 'NONE', #16878, #4420, #6891, .T. ) ;
#19639 = DIRECTION ( 'NONE',  ( -0.000000000000000000, -0.000000000000000000, 1.000000000000000000 ) ) ;
#19640 = DIRECTION ( 'NONE',  ( 1.000000000000000000, 9.912705577010325549E-17, 3.465149234233960866E-31 ) ) ;
#19641 = DIRECTION ( 'NONE',  ( 1.000000000000000000, 0.000000000000000000, 0.000000000000000000 ) ) ;
#19642 = LINE ( 'NONE', #3329, #2630 ) ;
#19643 = PLANE ( 'NONE',  #23479 ) ;
#19644 = DIRECTION ( 'NONE',  ( 1.000000000000000000, 0.000000000000000000, 0.000000000000000000 ) ) ;
#19645 = ORIENTED_EDGE ( 'NONE', *, *, #23057, .T. ) ;
#19646 = VERTEX_POINT ( 'NONE', #18668 ) ;
#19648 = VECTOR ( 'NONE', #224, 1000.000000000000000 ) ;
#19647 = AXIS2_PLACEMENT_3D ( 'NONE', #6793, #12152, #3160 ) ;
#19649 = DIRECTION ( 'NONE',  ( 1.000000000000000000, 0.000000000000000000, 0.000000000000000000 ) ) ;
#19650 = CARTESIAN_POINT ( 'NONE',  ( 280.9942590117597092, 268.9045205713625819, 146.9080393212557567 ) ) ;
#19651 = COLOUR_RGB ( '',0.8941176470588234615, 0.8941176470588234615, 0.8941176470588234615 ) ;
#19652 = AXIS2_PLACEMENT_3D ( 'NONE', #3779, #21788, #5254 ) ;
#19653 = ORIENTED_EDGE ( 'NONE', *, *, #9381, .F. ) ;
#19654 = VECTOR ( 'NONE', #5677, 1000.000000000000000 ) ;
#19655 = AXIS2_PLACEMENT_3D ( 'NONE', #13738, #11802, #2711 ) ;
#19656 = AXIS2_PLACEMENT_3D ( 'NONE', #5263, #9011, #17709 ) ;
#19657 = CARTESIAN_POINT ( 'NONE',  ( -146.0000000000001137, -494.4690652294807478, 27.94500000000641649 ) ) ;
#19658 = CARTESIAN_POINT ( 'NONE',  ( 2.699999999999997513, 2.467663300281916154E-15, 19.99999999999998934 ) ) ;
#19659 = EDGE_LOOP ( 'NONE', ( #16473, #17228 ) ) ;
#19660 = DIRECTION ( 'NONE',  ( 0.000000000000000000, 0.000000000000000000, 1.000000000000000000 ) ) ;
#19661 = DIRECTION ( 'NONE',  ( 0.000000000000000000, 0.000000000000000000, -1.000000000000000000 ) ) ;
#19662 = ORIENTED_EDGE ( 'NONE', *, *, #12855, .F. ) ;
#19663 = DIRECTION ( 'NONE',  ( 3.736327486719275871E-16, -1.000000000000000000, 3.469446951953614189E-15 ) ) ;
#19664 = ORIENTED_EDGE ( 'NONE', *, *, #3097, .T. ) ;
#19665 = PRODUCT_DEFINITION_FORMATION_WITH_SPECIFIED_SOURCE ( 'ANY', '', #3604, .NOT_KNOWN. ) ;
#19666 = DIRECTION ( 'NONE',  ( 0.000000000000000000, -1.000000000000000000, -5.286776307738891306E-15 ) ) ;
#19667 = COLOUR_RGB ( '',0.8941176470588234615, 0.8941176470588234615, 0.8941176470588234615 ) ;
#19669 = CIRCLE ( 'NONE', #23132, 2.649999999999985700 ) ;
#19668 = CARTESIAN_POINT ( 'NONE',  ( 2.500000000000002220, 1.768423874527826678, 1.020999999999997687 ) ) ;
#19670 = ORIENTED_EDGE ( 'NONE', *, *, #22868, .T. ) ;
#19671 = ORIENTED_EDGE ( 'NONE', *, *, #1340, .T. ) ;
#19672 = CARTESIAN_POINT ( 'NONE',  ( 133.8630869304077748, 78.13886732029796178, -31.53250949154611504 ) ) ;
#19673 = CONICAL_SURFACE ( 'NONE', #3860, 2.055000000000000160, 0.7853981633974633780 ) ;
#19674 = VECTOR ( 'NONE', #10347, 1000.000000000000000 ) ;
#19675 = DIRECTION ( 'NONE',  ( -0.1064154817287535221, -0.9943217513704692978, 1.303213790788408974E-17 ) ) ;
#19676 = PLANE ( 'NONE',  #21620 ) ;
#19677 = EDGE_CURVE ( 'NONE', #5510, #15457, #14122, .T. ) ;
#19678 = EDGE_CURVE ( 'NONE', #3554, #21032, #4179, .T. ) ;
#19679 = EDGE_CURVE ( 'NONE', #9606, #5897, #16454, .T. ) ;
#19680 = CARTESIAN_POINT ( 'NONE',  ( -5.112021521198522933, 5.708827036477257977, -7.069802615102034338 ) ) ;
#19681 = CYLINDRICAL_SURFACE ( 'NONE', #10937, 2.649999999999971934 ) ;
#19682 = ORIENTED_EDGE ( 'NONE', *, *, #20881, .T. ) ;
#19683 = CARTESIAN_POINT ( 'NONE',  ( 0.000000000000000000, 145.0000000000000284, -90.00000000000000000 ) ) ;
#19684 = FILL_AREA_STYLE ('',( #19318 ) ) ;
#19685 = ORIENTED_EDGE ( 'NONE', *, *, #2690, .F. ) ;
#19686 = CARTESIAN_POINT ( 'NONE',  ( -34.75000000000005684, 100.0000000000000000, 150.2000000000009550 ) ) ;
#19687 = ORIENTED_EDGE ( 'NONE', *, *, #10945, .F. ) ;
#19688 = LINE ( 'NONE', #14403, #8362 ) ;
#19689 = ORIENTED_EDGE ( 'NONE', *, *, #4493, .T. ) ;
#19690 = FACE_OUTER_BOUND ( 'NONE', #7658, .T. ) ;
#19691 = EDGE_LOOP ( 'NONE', ( #6311, #1556, #19140, #13656 ) ) ;
#19692 = DIRECTION ( 'NONE',  ( 0.000000000000000000, 0.000000000000000000, -1.000000000000000000 ) ) ;
#19693 = VERTEX_POINT ( 'NONE', #23148 ) ;
#19694 = DIRECTION ( 'NONE',  ( -0.000000000000000000, 0.8660254037844398178, 0.4999999999999980016 ) ) ;
#19695 = EDGE_CURVE ( 'NONE', #6907, #10894, #4916, .T. ) ;
#19696 = PRESENTATION_STYLE_ASSIGNMENT (( #23075 ) ) ;
#19697 = CARTESIAN_POINT ( 'NONE',  ( -24.99999999999998934, 45.00100000000041689, 64.99999999999984368 ) ) ;
#19698 = APPLICATION_CONTEXT ( 'automotive_design' ) ;
#19699 = CARTESIAN_POINT ( 'NONE',  ( 0.000000000000000000, -1.178949249685218970, -2.041999999999998483 ) ) ;
#19700 = ADVANCED_FACE ( 'NONE', ( #21583 ), #23383, .T. ) ;
#19701 = DIRECTION ( 'NONE',  ( 0.000000000000000000, 1.334402673828305746E-15, -1.000000000000000000 ) ) ;
#19702 = ORIENTED_EDGE ( 'NONE', *, *, #1911, .F. ) ;
#19703 = DIRECTION ( 'NONE',  ( 0.000000000000000000, 0.000000000000000000, 1.000000000000000000 ) ) ;
#19704 =( NAMED_UNIT ( * ) SI_UNIT ( $, .STERADIAN. ) SOLID_ANGLE_UNIT ( ) );
#19705 = PRODUCT_DEFINITION_SHAPE ( 'NONE', 'NONE',  #23831 ) ;
#19707 = ORIENTED_EDGE ( 'NONE', *, *, #13098, .F. ) ;
#19706 = ORIENTED_EDGE ( 'NONE', *, *, #16007, .F. ) ;
#19708 = DIRECTION ( 'NONE',  ( 1.000000000000000000, 0.000000000000000000, 0.000000000000000000 ) ) ;
#19709 = PLANE ( 'NONE',  #13151 ) ;
#19710 = FACE_OUTER_BOUND ( 'NONE', #10362, .T. ) ;
#19711 = CARTESIAN_POINT ( 'NONE',  ( 0.000000000000000000, 0.000000000000000000, 169.9999999999999716 ) ) ;
#19712 = CARTESIAN_POINT ( 'NONE',  ( 49.17200000000001836, 0.000000000000000000, 0.000000000000000000 ) ) ;
#19713 = ORIENTED_EDGE ( 'NONE', *, *, #16137, .T. ) ;
#19714 = CARTESIAN_POINT ( 'NONE',  ( -37.61698748598514896, -140.0355749532212428, 90.00000000000000000 ) ) ;
#19715 = VERTEX_POINT ( 'NONE', #3100 ) ;
#19716 = PLANE ( 'NONE',  #7689 ) ;
#19717 = CARTESIAN_POINT ( 'NONE',  ( -4.211140560182196957, -2.431303136016552013, -3.745885042887436178 ) ) ;
#19718 = CONTEXT_DEPENDENT_SHAPE_REPRESENTATION ( #5406, #14153 ) ;
#19719 = EDGE_CURVE ( 'NONE', #14837, #2779, #3396, .T. ) ;
#19720 = ORIENTED_EDGE ( 'NONE', *, *, #16990, .T. ) ;
#19721 = CYLINDRICAL_SURFACE ( 'NONE', #21772, 7.500000000000000000 ) ;
#19722 = VERTEX_POINT ( 'NONE', #12456 ) ;
#19723 = CARTESIAN_POINT ( 'NONE',  ( -7.263825692932299738, -4.945657111639584436, -7.907570769506049757 ) ) ;
#19724 = CYLINDRICAL_SURFACE ( 'NONE', #2540, 4.250000000000000000 ) ;
#19725 = EDGE_LOOP ( 'NONE', ( #5321, #17359, #6242 ) ) ;
#19726 = CARTESIAN_POINT ( 'NONE',  ( -7.500000000000000000, 4.330127018922191873, -10.00000000000000000 ) ) ;
#19727 = FILL_AREA_STYLE ('',( #23352 ) ) ;
#19728 = DIRECTION ( 'NONE',  ( 0.000000000000000000, -1.224646799147351975E-16, 1.000000000000000000 ) ) ;
#19729 = DIRECTION ( 'NONE',  ( 0.000000000000000000, -1.000000000000000000, 0.000000000000000000 ) ) ;
#19730 = DIRECTION ( 'NONE',  ( 0.000000000000000000, 1.177509268541832635E-16, -1.000000000000000000 ) ) ;
#19731 = LINE ( 'NONE', #8764, #7693 ) ;
#19732 = EDGE_CURVE ( 'NONE', #17846, #4308, #10614, .T. ) ;
#19733 = DIRECTION ( 'NONE',  ( 1.000000000000000000, -0.000000000000000000, 6.982962677686266711E-15 ) ) ;
#19734 = ORIENTED_EDGE ( 'NONE', *, *, #16570, .T. ) ;
#19735 =( NAMED_UNIT ( * ) PLANE_ANGLE_UNIT ( ) SI_UNIT ( $, .RADIAN. ) );
#19736 = LINE ( 'NONE', #19260, #10341 ) ;
#19737 = CARTESIAN_POINT ( 'NONE',  ( 4.999999999999999112, -5.773502691896267081, -7.063244554130005071 ) ) ;
#19738 = EDGE_CURVE ( 'NONE', #14650, #13361, #9591, .T. ) ;
#19739 = ORIENTED_EDGE ( 'NONE', *, *, #17752, .F. ) ;
#19740 = ORIENTED_EDGE ( 'NONE', *, *, #2690, .T. ) ;
#19741 = DIRECTION ( 'NONE',  ( 0.000000000000000000, 1.000000000000000000, 0.000000000000000000 ) ) ;
#19742 = LINE ( 'NONE', #17576, #20360 ) ;
#19743 =( REPRESENTATION_RELATIONSHIP ('NONE','NONE', #10127, #6236 ) REPRESENTATION_RELATIONSHIP_WITH_TRANSFORMATION ( #1485 )SHAPE_REPRESENTATION_RELATIONSHIP( ) );
#19744 = CARTESIAN_POINT ( 'NONE',  ( -282.6339272673398000, 272.3699028110927429, 145.4976310729378213 ) ) ;
#19745 = LINE ( 'NONE', #5140, #11527 ) ;
#19746 = CARTESIAN_POINT ( 'NONE',  ( -285.0335297745772323, 269.1488036478618824, -146.2439791848363768 ) ) ;
#19747 = VERTEX_POINT ( 'NONE', #3204 ) ;
#19748 = CARTESIAN_POINT ( 'NONE',  ( -146.0000000000005116, -494.4690652294800657, -29.99999999999356604 ) ) ;
#19749 = ORIENTED_EDGE ( 'NONE', *, *, #1310, .T. ) ;
#19750 = DIRECTION ( 'NONE',  ( -0.000000000000000000, -0.000000000000000000, 1.000000000000000000 ) ) ;
#19751 = CARTESIAN_POINT ( 'NONE',  ( -123.1824219776881648, 83.04955713735580503, -29.99999999999356248 ) ) ;
#19752 = LINE ( 'NONE', #19986, #20590 ) ;
#19753 = VERTEX_POINT ( 'NONE', #16150 ) ;
#19754 = DIRECTION ( 'NONE',  ( 0.000000000000000000, 1.000000000000000000, 0.000000000000000000 ) ) ;
#19755 = DIRECTION ( 'NONE',  ( 0.000000000000000000, -0.000000000000000000, 1.000000000000000000 ) ) ;
#19756 = ADVANCED_FACE ( 'NONE', ( #23511 ), #4557, .F. ) ;
#19757 = CARTESIAN_POINT ( 'NONE',  ( -20.00000000000000000, -1000.000000000000000, -150.0000000000000000 ) ) ;
#19758 = DIRECTION ( 'NONE',  ( -3.495664435217746987E-15, 1.000000000000000000, 0.000000000000000000 ) ) ;
#19759 = EDGE_CURVE ( 'NONE', #10258, #10166, #4683, .T. ) ;
#19760 = CARTESIAN_POINT ( 'NONE',  ( 0.000000000000000000, 2.357898499370432166, -2.385244779468109755E-15 ) ) ;
#19761 = DIRECTION ( 'NONE',  ( 0.9289202219288174023, 0.3702799228849934510, 6.982962677686266711E-15 ) ) ;
#19762 = CARTESIAN_POINT ( 'NONE',  ( -285.2000000000000455, 268.1431883596741841, 146.4301685938042112 ) ) ;
#19763 = VECTOR ( 'NONE', #4445, 1000.000000000000000 ) ;
#19764 = ORIENTED_EDGE ( 'NONE', *, *, #20135, .F. ) ;
#19765 = ORIENTED_EDGE ( 'NONE', *, *, #19836, .T. ) ;
#19766 = CARTESIAN_POINT ( 'NONE',  ( 10.00000000000000000, 0.000000000000000000, 0.000000000000000000 ) ) ;
#19767 = CARTESIAN_POINT ( 'NONE',  ( -155.0000000000000284, -784.4690652294798383, -29.99999999999350564 ) ) ;
#19768 = EDGE_CURVE ( 'NONE', #21871, #7027, #16534, .T. ) ;
#19769 = ORIENTED_EDGE ( 'NONE', *, *, #4035, .T. ) ;
#19770 = ADVANCED_FACE ( 'NONE', ( #19282 ), #15833, .F. ) ;
#19771 = CARTESIAN_POINT ( 'NONE',  ( -69.99999999999997158, -87.33333333333338544, 3.000000000000001332 ) ) ;
#19772 = DIRECTION ( 'NONE',  ( 0.000000000000000000, 0.000000000000000000, -1.000000000000000000 ) ) ;
#19773 = VERTEX_POINT ( 'NONE', #19637 ) ;
#19774 = CARTESIAN_POINT ( 'NONE',  ( 280.8708543776410806, 269.1333820183295416, 146.7350371479513171 ) ) ;
#19775 = EDGE_CURVE ( 'NONE', #2188, #6623, #2243, .T. ) ;
#19776 = DIRECTION ( 'NONE',  ( -0.000000000000000000, 1.000000000000000000, -0.000000000000000000 ) ) ;
#19777 = ORIENTED_EDGE ( 'NONE', *, *, #11829, .F. ) ;
#19778 = CARTESIAN_POINT ( 'NONE',  ( -134.5810953439730326, -1076.895678479287426, -30.65604281379823703 ) ) ;
#19779 = EDGE_CURVE ( 'NONE', #14699, #22322, #2749, .T. ) ;
#19780 = AXIS2_PLACEMENT_3D ( 'NONE', #3922, #18542, #560 ) ;
#19781 = MANIFOLD_SOLID_BREP ( 'Cavity1', #1735 ) ;
#19782 = VERTEX_POINT ( 'NONE', #13031 ) ;
#19783 = CARTESIAN_POINT ( 'NONE',  ( 45.00000000000000000, 250.0000000000000000, 0.000000000000000000 ) ) ;
#19784 = CARTESIAN_POINT ( 'NONE',  ( -194.7500000000004832, -784.4690652294792699, -29.99999999999322498 ) ) ;
#19785 = VERTEX_POINT ( 'NONE', #10732 ) ;
#19786 = ORIENTED_EDGE ( 'NONE', *, *, #995, .T. ) ;
#19787 = CARTESIAN_POINT ( 'NONE',  ( 133.6912351773694354, 78.43256762916455216, -28.11073331261974317 ) ) ;
#19788 = DIRECTION ( 'NONE',  ( 1.224646799147352468E-16, -8.300758060308986527E-32, -0.9999999999999998890 ) ) ;
#19789 = CARTESIAN_POINT ( 'NONE',  ( 0.000000000000000000, 145.0000000000000284, 90.00000000000000000 ) ) ;
#19790 = B_SPLINE_CURVE_WITH_KNOTS ( 'NONE', 3,
 ( #11250, #222, #2131, #11353, #18665, #3831 ),
 .UNSPECIFIED., .F., .F.,
 ( 4, 2, 4 ),
 ( 0.000000000000000000, 0.0002095117440854740156, 0.0004190234881709480313 ),
 .UNSPECIFIED. ) ;
#19791 = FACE_BOUND ( 'NONE', #3075, .T. ) ;
#19792 = CARTESIAN_POINT ( 'NONE',  ( 21.00000000000000355, 0.000000000000000000, 0.000000000000000000 ) ) ;
#19793 = CIRCLE ( 'NONE', #5520, 7.500000000000006217 ) ;
#19794 = EDGE_LOOP ( 'NONE', ( #20745, #14136, #890, #15978 ) ) ;
#19795 = EDGE_CURVE ( 'NONE', #5229, #8689, #8422, .T. ) ;
#19796 = CYLINDRICAL_SURFACE ( 'NONE', #9535, 2.649999999999985700 ) ;
#19797 =( NAMED_UNIT ( * ) SI_UNIT ( $, .STERADIAN. ) SOLID_ANGLE_UNIT ( ) );
#19798 = EDGE_CURVE ( 'NONE', #6258, #6350, #8136, .T. ) ;
#19799 = CONICAL_SURFACE ( 'NONE', #9398, 2.055000000000001492, 0.7853981633974633780 ) ;
#19800 = VERTEX_POINT ( 'NONE', #16276 ) ;
#19801 = EDGE_CURVE ( 'NONE', #15253, #12527, #5394, .T. ) ;
#19802 = FACE_OUTER_BOUND ( 'NONE', #5149, .T. ) ;
#19803 = DIRECTION ( 'NONE',  ( 1.000000000000000000, 0.000000000000000000, 0.000000000000000000 ) ) ;
#19804 = ADVANCED_FACE ( 'NONE', ( #10866 ), #7077, .F. ) ;
#19805 = ADVANCED_FACE ( 'NONE', ( #11221 ), #18292, .F. ) ;
#19806 = ORIENTED_EDGE ( 'NONE', *, *, #5230, .F. ) ;
#19808 = EDGE_CURVE ( 'NONE', #4703, #22432, #1865, .T. ) ;
#19807 = DIRECTION ( 'NONE',  ( 0.000000000000000000, 0.000000000000000000, -1.000000000000000000 ) ) ;
#19809 = AXIS2_PLACEMENT_3D ( 'NONE', #5650, #20493, #16876 ) ;
#19810 = ORIENTED_EDGE ( 'NONE', *, *, #19768, .T. ) ;
#19811 = PRODUCT_DEFINITION_SHAPE ( 'NONE', 'NONE',  #23814 ) ;
#19812 = CARTESIAN_POINT ( 'NONE',  ( 5.000000000000001776, 6.123233995736768255E-16, -9.974600000000000577 ) ) ;
#19813 = ORIENTED_EDGE ( 'NONE', *, *, #21980, .F. ) ;
#19814 = DIRECTION ( 'NONE',  ( 0.000000000000000000, -2.618450529776326854E-15, -1.000000000000000000 ) ) ;
#19815 = CARTESIAN_POINT ( 'NONE',  ( -280.8089314698395356, 269.2533442688712739, 146.6578961534456482 ) ) ;
#19816 = LINE ( 'NONE', #3266, #20742 ) ;
#19817 = MANIFOLD_SOLID_BREP ( 'Cut-Extrude-Thin2', #10257 ) ;
#19818 = DIRECTION ( 'NONE',  ( -1.000000000000000000, -0.000000000000000000, -0.000000000000000000 ) ) ;
#19819 = DIRECTION ( 'NONE',  ( -1.000000000000000000, 0.000000000000000000, 0.000000000000000000 ) ) ;
#19820 = VERTEX_POINT ( 'NONE', #16627 ) ;
#19821 = CARTESIAN_POINT ( 'NONE',  ( 2.500000000000000000, 1.178949249685212974, -2.042000000000001148 ) ) ;
#19822 =( GEOMETRIC_REPRESENTATION_CONTEXT ( 3 ) GLOBAL_UNCERTAINTY_ASSIGNED_CONTEXT ( ( #8082 ) ) GLOBAL_UNIT_ASSIGNED_CONTEXT ( ( #15917, #10864, #6725 ) ) REPRESENTATION_CONTEXT ( 'NONE', 'WORKASPACE' ) );
#19824 = VERTEX_POINT ( 'NONE', #23728 ) ;
#19823 = VERTEX_POINT ( 'NONE', #12811 ) ;
#19825 = VECTOR ( 'NONE', #12537, 1000.000000000000114 ) ;
#19826 = DIRECTION ( 'NONE',  ( 6.123233995736766036E-17, 0.000000000000000000, -1.000000000000000000 ) ) ;
#19827 = DIRECTION ( 'NONE',  ( 0.000000000000000000, 1.000000000000000000, -1.224646799147353207E-16 ) ) ;
#19828 = CARTESIAN_POINT ( 'NONE',  ( -122.8605704798723082, 82.74225173005861222, 30.00000000000641620 ) ) ;
#19829 = AXIS2_PLACEMENT_3D ( 'NONE', #8096, #4935, #1059 ) ;
#19830 = FACE_OUTER_BOUND ( 'NONE', #10847, .T. ) ;
#19831 = CARTESIAN_POINT ( 'NONE',  ( 2.500000000000002220, -1.178949249685215417, 2.042000000000002036 ) ) ;
#19832 = EDGE_CURVE ( 'NONE', #22779, #10209, #8120, .T. ) ;
#19833 = VERTEX_POINT ( 'NONE', #3670 ) ;
#19834 = ADVANCED_FACE ( 'NONE', ( #11085 ), #22511, .F. ) ;
#19835 = CARTESIAN_POINT ( 'NONE',  ( 45.00000000000000711, 5.510910596163090344E-15, 20.00000000000000000 ) ) ;
#19836 = EDGE_CURVE ( 'NONE', #223, #9869, #6101, .T. ) ;
#19837 = ORIENTED_EDGE ( 'NONE', *, *, #18779, .T. ) ;
#19838 = CIRCLE ( 'NONE', #8287, 0.2500000000000002220 ) ;
#19839 = CARTESIAN_POINT ( 'NONE',  ( 24.99999999999998224, -1000.000000000000000, -145.0000119999999697 ) ) ;
#19840 = CARTESIAN_POINT ( 'NONE',  ( 20.00000000000000000, 0.000000000000000000, 138.9999999999999716 ) ) ;
#19841 = ITEM_DEFINED_TRANSFORMATION ( 'NONE', 'NONE', #7731,  #11210 ) ;
#19842 = ORIENTED_EDGE ( 'NONE', *, *, #12011, .T. ) ;
#19843 = ORIENTED_EDGE ( 'NONE', *, *, #19, .F. ) ;
#19844 = DIRECTION ( 'NONE',  ( 0.6964005597823107463, -0.7176533009294140397, 6.982962677686265922E-15 ) ) ;
#19845 = VECTOR ( 'NONE', #6691, 1000.000000000000000 ) ;
#19846 = CARTESIAN_POINT ( 'NONE',  ( 0.000000000000000000, 0.000000000000000000, 100.0000000000000000 ) ) ;
#19847 = EDGE_LOOP ( 'NONE', ( #22968, #10907, #13212, #13023, #11623, #22761 ) ) ;
#19848 = LINE ( 'NONE', #19959, #13288 ) ;
#19849 = CARTESIAN_POINT ( 'NONE',  ( 133.6256533058501077, 78.54427823740881820, 28.00660068667233560 ) ) ;
#19850 = AXIS2_PLACEMENT_3D ( 'NONE', #13317, #489, #14991 ) ;
#19851 = CARTESIAN_POINT ( 'NONE',  ( -2.999999999999995559, 0.000000000000000000, -21.50000000000000000 ) ) ;
#19852 = CIRCLE ( 'NONE', #15254, 5.249999999999949374 ) ;
#19853 = DIRECTION ( 'NONE',  ( 1.000000000000000000, 0.000000000000000000, 0.000000000000000000 ) ) ;
#19854 = DIRECTION ( 'NONE',  ( -1.000000000000000000, 0.000000000000000000, -0.000000000000000000 ) ) ;
#19855 = DIRECTION ( 'NONE',  ( -0.000000000000000000, -0.000000000000000000, 1.000000000000000000 ) ) ;
#19856 = CARTESIAN_POINT ( 'NONE',  ( -105.0000000000000142, 30.00000000000001421, 0.000000000000000000 ) ) ;
#19857 = ORIENTED_EDGE ( 'NONE', *, *, #17099, .F. ) ;
#19858 = LINE ( 'NONE', #14446, #17657 ) ;
#19859 = CARTESIAN_POINT ( 'NONE',  ( -1.360585162435467455, 4.061296242128285883, -3.505054077164959203 ) ) ;
#19860 = EDGE_LOOP ( 'NONE', ( #22360, #19570, #2645, #15222 ) ) ;
#19861 = CIRCLE ( 'NONE', #9463, 0.5155456020628804703 ) ;
#19862 = DIRECTION ( 'NONE',  ( -0.7071067811865416886, 9.961996129952529179E-15, -0.7071067811865532349 ) ) ;
#19863 = LINE ( 'NONE', #18178, #21066 ) ;
#19864 = CARTESIAN_POINT ( 'NONE',  ( -280.6847249064869629, 273.0299999999999159, 145.1244295015775947 ) ) ;
#19865 = VECTOR ( 'NONE', #8572, 1000.000000000000000 ) ;
#19866 = ADVANCED_FACE ( 'NONE', ( #13388 ), #2470, .F. ) ;
#19867 = DIRECTION ( 'NONE',  ( -0.7232617928448825673, 0.6905739489807055653, 6.982962677686265922E-15 ) ) ;
#19868 = FACE_OUTER_BOUND ( 'NONE', #5691, .T. ) ;
#19869 = ORIENTED_EDGE ( 'NONE', *, *, #20472, .T. ) ;
#19870 = DIRECTION ( 'NONE',  ( 1.000000000000000000, -0.000000000000000000, 6.982962677686266711E-15 ) ) ;
#19871 = ORIENTED_EDGE ( 'NONE', *, *, #1850, .T. ) ;
#19872 = DIRECTION ( 'NONE',  ( -0.000000000000000000, -0.000000000000000000, -1.000000000000000000 ) ) ;
#19873 = DIRECTION ( 'NONE',  ( -0.000000000000000000, 1.000000000000000000, 0.000000000000000000 ) ) ;
#19874 = CIRCLE ( 'NONE', #20617, 2.499999999999998668 ) ;
#19875 = VERTEX_POINT ( 'NONE', #18893 ) ;
#19876 = CARTESIAN_POINT ( 'NONE',  ( -281.4928932188134922, -132.2000000000000455, -7.703011046602857601E-15 ) ) ;
#19877 = CARTESIAN_POINT ( 'NONE',  ( 2.500000000000002220, -2.357898499370430834, 3.469446951953614189E-15 ) ) ;
#19878 = FACE_BOUND ( 'NONE', #7001, .T. ) ;
#19879 = CARTESIAN_POINT ( 'NONE',  ( -7.922281120364393914, 4.573931137438271399, -8.047472243342930653 ) ) ;
#19880 = DIRECTION ( 'NONE',  ( -0.000000000000000000, 0.000000000000000000, 1.000000000000000000 ) ) ;
#19881 = DIRECTION ( 'NONE',  ( 0.000000000000000000, 0.000000000000000000, -1.000000000000000000 ) ) ;
#19882 = CIRCLE ( 'NONE', #2134, 2.649999999999971934 ) ;
#19883 = CIRCLE ( 'NONE', #5558, 2.499999999999998668 ) ;
#19884 = VERTEX_POINT ( 'NONE', #18759 ) ;
#19885 = VERTEX_POINT ( 'NONE', #2105 ) ;
#19886 = DIRECTION ( 'NONE',  ( 0.9289202219288174023, 0.3702799228849934510, 6.982962677686266711E-15 ) ) ;
#19887 = DIRECTION ( 'NONE',  ( 0.000000000000000000, 0.000000000000000000, -1.000000000000000000 ) ) ;
#19888 = VERTEX_POINT ( 'NONE', #2587 ) ;
#19889 = CARTESIAN_POINT ( 'NONE',  ( -194.7500000000000284, -494.4690652294800657, 30.00000000000675726 ) ) ;
#19890 = CARTESIAN_POINT ( 'NONE',  ( 2.558993250143296372, -7.638875775590942219, -7.593821156097518177 ) ) ;
#19891 = AXIS2_PLACEMENT_3D ( 'NONE', #22893, #23142, #6363 ) ;
#19892 = VERTEX_POINT ( 'NONE', #17217 ) ;
#19893 = ADVANCED_FACE ( 'NONE', ( #11575 ), #11446, .T. ) ;
#19894 = LINE ( 'NONE', #21608, #2576 ) ;
#19895 = ORIENTED_EDGE ( 'NONE', *, *, #11687, .T. ) ;
#19896 = DIRECTION ( 'NONE',  ( 1.000000000000000000, -0.000000000000000000, 0.000000000000000000 ) ) ;
#19897 = EDGE_CURVE ( 'NONE', #15868, #1963, #22270, .T. ) ;
#19898 = EDGE_CURVE ( 'NONE', #6562, #1031, #18090, .T. ) ;
#19899 = VECTOR ( 'NONE', #22596, 1000.000000000000000 ) ;
#19900 = ORIENTED_EDGE ( 'NONE', *, *, #21375, .T. ) ;
#19901 = DIRECTION ( 'NONE',  ( 0.000000000000000000, 0.000000000000000000, 1.000000000000000000 ) ) ;
#19902 = DIRECTION ( 'NONE',  ( -0.000000000000000000, -0.000000000000000000, 1.000000000000000000 ) ) ;
#19903 = EDGE_CURVE ( 'NONE', #20959, #4361, #17699, .T. ) ;
#19904 = CARTESIAN_POINT ( 'NONE',  ( -4.024497503033519941, 2.323544716729375459, -3.572167766733379768 ) ) ;
#19905 = ORIENTED_EDGE ( 'NONE', *, *, #21692, .T. ) ;
#19906 = EDGE_LOOP ( 'NONE', ( #3362, #8400, #10242, #13878 ) ) ;
#19907 = DIRECTION ( 'NONE',  ( -0.6663528160696001734, -0.2365880903936319335, -0.7071067811865532349 ) ) ;
#19908 = PRODUCT_DEFINITION_SHAPE ( 'NONE', 'NONE',  #23825 ) ;
#19909 = CARTESIAN_POINT ( 'NONE',  ( 40.00000000000000711, 100.0000000000000000, -114.9999999999999574 ) ) ;
#19910 = CARTESIAN_POINT ( 'NONE',  ( -126.4560199014025414, 89.63188623867986848, -29.83733181946746527 ) ) ;
#19911 = AXIS2_PLACEMENT_3D ( 'NONE', #15161, #293, #2338 ) ;
#19912 = LINE ( 'NONE', #7221, #16616 ) ;
#19913 = DIRECTION ( 'NONE',  ( -0.000000000000000000, -0.000000000000000000, 1.000000000000000000 ) ) ;
#19914 = EDGE_CURVE ( 'NONE', #23021, #20709, #8084, .T. ) ;
#19915 = ORIENTED_EDGE ( 'NONE', *, *, #17353, .T. ) ;
#19916 = VECTOR ( 'NONE', #15053, 1000.000000000000000 ) ;
#19917 = DIRECTION ( 'NONE',  ( -0.6663528160696001734, -0.2365880903936319335, -0.7071067811865532349 ) ) ;
#19918 =( NAMED_UNIT ( * ) PLANE_ANGLE_UNIT ( ) SI_UNIT ( $, .RADIAN. ) );
#19919 = CARTESIAN_POINT ( 'NONE',  ( -146.4450000000000784, -494.4690652294807478, 30.00000000000641975 ) ) ;
#19920 = CARTESIAN_POINT ( 'NONE',  ( -100.0000000000000000, 270.0000000000000000, -144.9999999999999716 ) ) ;
#19921 = ORIENTED_EDGE ( 'NONE', *, *, #8485, .F. ) ;
#19922 = AXIS2_PLACEMENT_3D ( 'NONE', #14323, #46, #18367 ) ;
#19923 = CARTESIAN_POINT ( 'NONE',  ( 1.282512619718868541, 8.391164935524033197, -7.795653906408837486 ) ) ;
#19924 = FACE_OUTER_BOUND ( 'NONE', #1544, .T. ) ;
#19925 = ORIENTED_EDGE ( 'NONE', *, *, #22741, .T. ) ;
#19926 = DIRECTION ( 'NONE',  ( -1.000000000000000000, -0.000000000000000000, -0.000000000000000000 ) ) ;
#19927 = EDGE_CURVE ( 'NONE', #13438, #21770, #6228, .T. ) ;
#19928 = VERTEX_POINT ( 'NONE', #15425 ) ;
#19929 = EDGE_CURVE ( 'NONE', #3142, #8675, #22767, .T. ) ;
#19930 = CARTESIAN_POINT ( 'NONE',  ( 1.734723475976807094E-15, 4.618802153517012954, -0.4999999999999995559 ) ) ;
#19931 = AXIS2_PLACEMENT_3D ( 'NONE', #15955, #14161, #21490 ) ;
#19932 = FACE_OUTER_BOUND ( 'NONE', #6320, .T. ) ;
#19933 = PLANE ( 'NONE',  #20142 ) ;
#19934 = EDGE_CURVE ( 'NONE', #9824, #12957, #11814, .T. ) ;
#19935 = FACE_OUTER_BOUND ( 'NONE', #5509, .T. ) ;
#19936 = ORIENTED_EDGE ( 'NONE', *, *, #17201, .T. ) ;
#19937 = FACE_OUTER_BOUND ( 'NONE', #17597, .T. ) ;
#19938 = AXIS2_PLACEMENT_3D ( 'NONE', #9909, #12110, #1060 ) ;
#19939 = ADVANCED_FACE ( 'NONE', ( #15066 ), #2355, .F. ) ;
#19941 = EDGE_LOOP ( 'NONE', ( #5638, #2236, #23760, #264 ) ) ;
#19940 = EDGE_LOOP ( 'NONE', ( #8972, #4439, #1360, #15937 ) ) ;
#19942 = CARTESIAN_POINT ( 'NONE',  ( -44.99999999999995737, -47.79999999999969873, 250.0000000000002274 ) ) ;
#19943 = DIRECTION ( 'NONE',  ( 1.000000000000000000, 0.000000000000000000, 0.000000000000000000 ) ) ;
#19944 = FACE_OUTER_BOUND ( 'NONE', #7893, .T. ) ;
#19945 = ORIENTED_EDGE ( 'NONE', *, *, #4335, .F. ) ;
#19946 = LINE ( 'NONE', #18253, #1006 ) ;
#19947 = CIRCLE ( 'NONE', #2202, 7.500000000000000888 ) ;
#19948 = DIRECTION ( 'NONE',  ( 5.050510105632271307E-15, -4.822252111914687128E-15, 1.000000000000000000 ) ) ;
#19949 = VERTEX_POINT ( 'NONE', #7914 ) ;
#19950 = CONICAL_SURFACE ( 'NONE', #9556, 2.055000000000000160, 0.7853981633974794763 ) ;
#19951 = CARTESIAN_POINT ( 'NONE',  ( 80.00000000000001421, -59.79999999999913030, 250.0000000000000000 ) ) ;
#19952 = DIRECTION ( 'NONE',  ( -3.469446951953614682E-16, 1.000000000000000000, -3.491481338843133355E-15 ) ) ;
#19953 = CIRCLE ( 'NONE', #21121, 20.00000000000000000 ) ;
#19954 = ITEM_DEFINED_TRANSFORMATION ( 'NONE', 'NONE', #21612,  #11210 ) ;
#19955 = ORIENTED_EDGE ( 'NONE', *, *, #515, .T. ) ;
#19956 = ORIENTED_EDGE ( 'NONE', *, *, #18903, .T. ) ;
#19957 = CYLINDRICAL_SURFACE ( 'NONE', #7155, 2.100000000000000089 ) ;
#19958 = ORIENTED_EDGE ( 'NONE', *, *, #14539, .F. ) ;
#19959 = CARTESIAN_POINT ( 'NONE',  ( 93.00000000000000000, -74.99999999999998579, 0.000000000000000000 ) ) ;
#19960 = CARTESIAN_POINT ( 'NONE',  ( 133.6917068022185617, 78.43176171823573384, 28.11170275877340785 ) ) ;
#19961 = CARTESIAN_POINT ( 'NONE',  ( 0.6937372685066666156, -4.453844082567737672, -3.610536846335894445 ) ) ;
#19962 = FACE_OUTER_BOUND ( 'NONE', #12129, .T. ) ;
#19963 = EDGE_CURVE ( 'NONE', #11453, #21308, #20389, .T. ) ;
#19964 = ADVANCED_FACE ( 'NONE', ( #13269 ), #20577, .F. ) ;
#19965 = CARTESIAN_POINT ( 'NONE',  ( 0.000000000000000000, 0.000000000000000000, -0.5776712190230133270 ) ) ;
#19966 = EDGE_CURVE ( 'NONE', #15661, #21242, #16986, .T. ) ;
#19967 = DIRECTION ( 'NONE',  ( 1.000000000000000000, 0.000000000000000000, 0.000000000000000000 ) ) ;
#19968 = AXIS2_PLACEMENT_3D ( 'NONE', #20121, #7086, #14474 ) ;
#19969 = VERTEX_POINT ( 'NONE', #13522 ) ;
#19970 = DIRECTION ( 'NONE',  ( -1.000000000000000000, -2.775557561562891351E-17, 0.000000000000000000 ) ) ;
#19971 = AXIS2_PLACEMENT_3D ( 'NONE', #11241, #11347, #18553 ) ;
#19972 = DIRECTION ( 'NONE',  ( 0.000000000000000000, 0.000000000000000000, 1.000000000000000000 ) ) ;
#19973 = AXIS2_PLACEMENT_3D ( 'NONE', #5019, #10705, #17812 ) ;
#19974 = VERTEX_POINT ( 'NONE', #20838 ) ;
#19975 = CARTESIAN_POINT ( 'NONE',  ( 155.0000000000000284, -209.9999999999996874, 30.00000000000648015 ) ) ;
#19976 = CARTESIAN_POINT ( 'NONE',  ( 0.000000000000000000, -1000.000000000000000, -145.0000119999999697 ) ) ;
#19977 = CARTESIAN_POINT ( 'NONE',  ( -284.1582675804706355, 270.9956429438695409, 145.8708543776411659 ) ) ;
#19978 = CARTESIAN_POINT ( 'NONE',  ( 0.000000000000000000, -1000.000000000000000, -138.9999999999999716 ) ) ;
#19979 = DIRECTION ( 'NONE',  ( -6.753181414994864868E-15, 6.753181414994864868E-15, -1.000000000000000000 ) ) ;
#19980 = EDGE_LOOP ( 'NONE', ( #17836, #1429 ) ) ;
#19981 = DIRECTION ( 'NONE',  ( -1.000000000000000000, -2.775557561562891351E-17, 0.000000000000000000 ) ) ;
#19982 = ORIENTED_EDGE ( 'NONE', *, *, #7802, .T. ) ;
#19984 = DIRECTION ( 'NONE',  ( 0.000000000000000000, 0.000000000000000000, -1.000000000000000000 ) ) ;
#19983 = VECTOR ( 'NONE', #694, 1000.000000000000000 ) ;
#19985 = CARTESIAN_POINT ( 'NONE',  ( 7.499999999999999112, 0.000000000000000000, 100.0000000000000000 ) ) ;
#19986 = CARTESIAN_POINT ( 'NONE',  ( 155.0000000000000284, -500.0000000000000000, -27.49999999999996803 ) ) ;
#19987 = CIRCLE ( 'NONE', #21151, 2.055000000000001492 ) ;
#19988 = ORIENTED_EDGE ( 'NONE', *, *, #16570, .F. ) ;
#19989 = FILL_AREA_STYLE_COLOUR ( '', #21147 ) ;
#19990 = AXIS2_PLACEMENT_3D ( 'NONE', #11786, #19215, #9833 ) ;
#19991 = LINE ( 'NONE', #3796, #1083 ) ;
#19992 = DIRECTION ( 'NONE',  ( -3.469446951953614682E-16, 1.000000000000000000, -3.491481338843133355E-15 ) ) ;
#19993 = DIRECTION ( 'NONE',  ( -0.000000000000000000, 1.000000000000000000, -3.469446951953613794E-15 ) ) ;
#19994 = CARTESIAN_POINT ( 'NONE',  ( -282.2000000000008981, 30.00000000000101963, -107.6499999999999773 ) ) ;
#19995 = CARTESIAN_POINT ( 'NONE',  ( -24.99999999999998934, 45.00100000000031031, 34.99999999999983658 ) ) ;
#19996 = VECTOR ( 'NONE', #2614, 1000.000000000000000 ) ;
#19997 = CARTESIAN_POINT ( 'NONE',  ( 12.52876685377502675, 21.69578997558840427, 145.0000119999999981 ) ) ;
#19998 = ORIENTED_EDGE ( 'NONE', *, *, #2696, .T. ) ;
#19999 = ORIENTED_EDGE ( 'NONE', *, *, #14592, .F. ) ;
#20000 = DIRECTION ( 'NONE',  ( 1.110223024625155594E-14, 0.000000000000000000, -1.000000000000000000 ) ) ;
#20001 = CARTESIAN_POINT ( 'NONE',  ( -52.99999999999997158, -130.5567675943147208, 0.000000000000000000 ) ) ;
#20002 = ORIENTED_EDGE ( 'NONE', *, *, #21945, .T. ) ;
#20003 = PRODUCT ( 'head pulley', 'head pulley', '', ( #21099 ) ) ;
#20004 = CARTESIAN_POINT ( 'NONE',  ( 9.787707486204086038, 2.366756136221725981, 200.0000120000000265 ) ) ;
#20005 = CARTESIAN_POINT ( 'NONE',  ( 0.9763930676190096802, -8.096533237419681228, -7.213065638943101376 ) ) ;
#20006 = VECTOR ( 'NONE', #5246, 1000.000000000000000 ) ;
#20007 = VECTOR ( 'NONE', #9754, 1000.000000000000114 ) ;
#20008 = CONICAL_SURFACE ( 'NONE', #7288, 4.000000000000000000, 0.8911886515913786111 ) ;
#20009 = AXIS2_PLACEMENT_3D ( 'NONE', #14128, #3106, #10508 ) ;
#20010 = ORIENTED_EDGE ( 'NONE', *, *, #17140, .F. ) ;
#20011 = DIRECTION ( 'NONE',  ( 0.000000000000000000, -1.000000000000000000, 0.000000000000000000 ) ) ;
#20012 = MECHANICAL_DESIGN_GEOMETRIC_PRESENTATION_REPRESENTATION (  '', ( #18476 ), #8092 ) ;
#20013 = CARTESIAN_POINT ( 'NONE',  ( 3.750000000000005329, 6.495190528383288253, 0.000000000000000000 ) ) ;
#20014 = ORIENTED_EDGE ( 'NONE', *, *, #20563, .T. ) ;
#20015 = DIRECTION ( 'NONE',  ( 3.202566417187928841E-16, -1.000000000000000000, 3.469446951953614583E-15 ) ) ;
#20016 =( REPRESENTATION_RELATIONSHIP ('NONE','NONE', #10127, #18083 ) REPRESENTATION_RELATIONSHIP_WITH_TRANSFORMATION ( #9850 )SHAPE_REPRESENTATION_RELATIONSHIP( ) );
#20017 = MANIFOLD_SOLID_BREP ( 'M5 Clearance Hole1', #589 ) ;
#20018 = ORIENTED_EDGE ( 'NONE', *, *, #3031, .T. ) ;
#20019 = CARTESIAN_POINT ( 'NONE',  ( -280.0000000000000568, 269.9999999999999432, -144.9999999999999716 ) ) ;
#20020 = CARTESIAN_POINT ( 'NONE',  ( -44.99999999999995026, -52.79999999999969873, 50.00000000000018474 ) ) ;
#20021 = CIRCLE ( 'NONE', #12748, 2.649999999999971934 ) ;
#20022 = DIRECTION ( 'NONE',  ( -0.8191520442889907994, 1.003171929053523514E-16, 0.5735764363510474917 ) ) ;
#20023 = VERTEX_POINT ( 'NONE', #14207 ) ;
#20024 = ORIENTED_EDGE ( 'NONE', *, *, #6927, .T. ) ;
#20025 = EDGE_CURVE ( 'NONE', #20656, #12219, #2261, .T. ) ;
#20026 = DIRECTION ( 'NONE',  ( 0.000000000000000000, 0.000000000000000000, 1.000000000000000000 ) ) ;
#20027 = VECTOR ( 'NONE', #9467, 1000.000000000000000 ) ;
#20028 = CARTESIAN_POINT ( 'NONE',  ( 5.000000000000000000, 0.000000000000000000, 0.000000000000000000 ) ) ;
#20029 = VECTOR ( 'NONE', #19844, 1000.000000000000114 ) ;
#20030 = AXIS2_PLACEMENT_3D ( 'NONE', #5328, #22343, #3869 ) ;
#20032 = CARTESIAN_POINT ( 'NONE',  ( 0.000000000000000000, 0.000000000000000000, -0.5776712190230133270 ) ) ;
#20031 = VECTOR ( 'NONE', #9358, 1000.000000000000000 ) ;
#20033 = CIRCLE ( 'NONE', #3819, 2.649999999999999467 ) ;
#20034 = DIRECTION ( 'NONE',  ( 0.000000000000000000, 1.177509268541832635E-16, -1.000000000000000000 ) ) ;
#20035 = AXIS2_PLACEMENT_3D ( 'NONE', #22499, #657, #22855 ) ;
#20036 = AXIS2_PLACEMENT_3D ( 'NONE', #14458, #19981, #8655 ) ;
#20037 = ADVANCED_FACE ( 'NONE', ( #1259 ), #21421, .F. ) ;
#20038 = ORIENTED_EDGE ( 'NONE', *, *, #14212, .T. ) ;
#20039 = CARTESIAN_POINT ( 'NONE',  ( 16.52066876451828392, -18.83467029480908295, 145.0000119999999697 ) ) ;
#20040 = ADVANCED_FACE ( 'NONE', ( #17454 ), #19600, .F. ) ;
#20041 = EDGE_CURVE ( 'NONE', #8456, #10894, #5016, .T. ) ;
#20042 = DIRECTION ( 'NONE',  ( -1.000000000000000000, 1.408839003528726857E-14, 6.982962677686266711E-15 ) ) ;
#20043 = CARTESIAN_POINT ( 'NONE',  ( 0.000000000000000000, 0.000000000000000000, 0.000000000000000000 ) ) ;
#20045 = AXIS2_PLACEMENT_3D ( 'NONE', #10248, #21097, #8551 ) ;
#20044 = AXIS2_PLACEMENT_3D ( 'NONE', #3392, #3036, #17793 ) ;
#20046 = ORIENTED_EDGE ( 'NONE', *, *, #7564, .T. ) ;
#20047 = B_SPLINE_CURVE_WITH_KNOTS ( 'NONE', 3,
 ( #1341, #10794, #16087, #6666, #14062, #21389 ),
 .UNSPECIFIED., .F., .F.,
 ( 4, 2, 4 ),
 ( 0.000000000000000000, 0.0004189869898914143787, 0.0008379739797828287574 ),
 .UNSPECIFIED. ) ;
#20048 = CARTESIAN_POINT ( 'NONE',  ( -0.04725809328185606034, 9.175759667312519241, -8.057670357645360326 ) ) ;
#20049 = VECTOR ( 'NONE', #1973, 1000.000000000000000 ) ;
#20050 = VECTOR ( 'NONE', #16678, 1000.000000000000000 ) ;
#20051 = AXIS2_PLACEMENT_3D ( 'NONE', #18772, #6114, #11707 ) ;
#20052 = ORIENTED_EDGE ( 'NONE', *, *, #21109, .T. ) ;
#20053 = CARTESIAN_POINT ( 'NONE',  ( -137.9031948627974486, 44.80746418436699940, -90.00000000000000000 ) ) ;
#20054 = ORIENTED_EDGE ( 'NONE', *, *, #3209, .F. ) ;
#20055 = CIRCLE ( 'NONE', #3025, 9.999999999999998224 ) ;
#20056 = DIRECTION ( 'NONE',  ( 1.000000000000000000, 0.000000000000000000, 0.000000000000000000 ) ) ;
#20057 = CARTESIAN_POINT ( 'NONE',  ( 16.52066876451827326, -1018.834670294808802, 145.0000119999999697 ) ) ;
#20058 = DIRECTION ( 'NONE',  ( 0.000000000000000000, 0.000000000000000000, 1.000000000000000000 ) ) ;
#20059 = MANIFOLD_SOLID_BREP ( 'Hex', #20629 ) ;
#20060 = CARTESIAN_POINT ( 'NONE',  ( -123.1824219776881648, 83.04955713735579081, -27.49999999999356248 ) ) ;
#20061 = DIRECTION ( 'NONE',  ( -1.000000000000000000, -0.000000000000000000, -0.000000000000000000 ) ) ;
#20062 = VERTEX_POINT ( 'NONE', #4525 ) ;
#20063 = PRODUCT_DEFINITION_FORMATION_WITH_SPECIFIED_SOURCE ( 'ANY', '', #13866, .NOT_KNOWN. ) ;
#20064 = DIRECTION ( 'NONE',  ( 0.000000000000000000, -1.224646799147353454E-16, 1.000000000000000000 ) ) ;
#20065 = SHAPE_REPRESENTATION_RELATIONSHIP ( 'NONE' , 'NONE' ,  #15622, #19351 ) ;
#20066 = VECTOR ( 'NONE', #11730, 1000.000000000000000 ) ;
#20067 = CIRCLE ( 'NONE', #9680, 4.057500000000000107 ) ;
#20069 = ORIENTED_EDGE ( 'NONE', *, *, #7652, .T. ) ;
#20068 = ORIENTED_EDGE ( 'NONE', *, *, #18003, .F. ) ;
#20070 = CARTESIAN_POINT ( 'NONE',  ( -293.2000000000010118, 34.99999999999915445, 105.0000000000002842 ) ) ;
#20071 = LINE ( 'NONE', #11042, #3840 ) ;
#20072 = CARTESIAN_POINT ( 'NONE',  ( 146.0000000000001990, -801.0618695410406644, -27.94499999999356632 ) ) ;
#20073 = EDGE_CURVE ( 'NONE', #11805, #10493, #10585, .T. ) ;
#20074 = EDGE_LOOP ( 'NONE', ( #10038, #9751, #9590 ) ) ;
#20075 = EDGE_CURVE ( 'NONE', #14004, #18956, #23114, .T. ) ;
#20076 = DIRECTION ( 'NONE',  ( 0.000000000000000000, -1.177509268541832635E-16, 1.000000000000000000 ) ) ;
#20077 = DIRECTION ( 'NONE',  ( 3.469446951953614682E-16, -1.000000000000000000, 3.483493295888648978E-15 ) ) ;
#20078 = EDGE_CURVE ( 'NONE', #11951, #17193, #19476, .T. ) ;
#20079 = VERTEX_POINT ( 'NONE', #1141 ) ;
#20080 = CARTESIAN_POINT ( 'NONE',  ( -45.00000000000000711, 0.000000000000000000, 169.9999999999999716 ) ) ;
#20081 = CARTESIAN_POINT ( 'NONE',  ( 2.290893957444128645E-15, 4.647089433458768681, -3.572167766733382877 ) ) ;
#20082 = ADVANCED_FACE ( 'NONE', ( #6454 ), #22017, .F. ) ;
#20083 = ITEM_DEFINED_TRANSFORMATION ( 'NONE', 'NONE', #22368,  #11210 ) ;
#20084 = ORIENTED_EDGE ( 'NONE', *, *, #1145, .T. ) ;
#20085 = EDGE_LOOP ( 'NONE', ( #23391, #13289, #16386, #9629 ) ) ;
#20086 = CARTESIAN_POINT ( 'NONE',  ( -160.0000000000000000, 0.000000000000000000, -90.00000000000000000 ) ) ;
#20087 = ORIENTED_EDGE ( 'NONE', *, *, #9156, .F. ) ;
#20088 = CARTESIAN_POINT ( 'NONE',  ( 24.19924082444365254, -993.5122791911473996, -145.0000000000000568 ) ) ;
#20089 = CARTESIAN_POINT ( 'NONE',  ( 133.0106877214035137, 79.58129789419636779, 32.48389983298810790 ) ) ;
#20090 = CARTESIAN_POINT ( 'NONE',  ( 4.000000000000000000, -0.8732470631449981147, -3.223155494240760088 ) ) ;
#20091 = FACE_OUTER_BOUND ( 'NONE', #6060, .T. ) ;
#20092 = DIRECTION ( 'NONE',  ( 0.000000000000000000, 0.4999999999999992784, -0.8660254037844390407 ) ) ;
#20093 = CARTESIAN_POINT ( 'NONE',  ( 155.0000000000000568, -801.0618695410406644, -27.49999999999350209 ) ) ;
#20094 = ORIENTED_EDGE ( 'NONE', *, *, #14191, .F. ) ;
#20095 = DIRECTION ( 'NONE',  ( 0.000000000000000000, 0.000000000000000000, 1.000000000000000000 ) ) ;
#20096 = EDGE_CURVE ( 'NONE', #12624, #2756, #10943, .T. ) ;
#20097 = CARTESIAN_POINT ( 'NONE',  ( -7.500000000000000000, 1.854554393013821745, -0.1880126015361722192 ) ) ;
#20098 = CYLINDRICAL_SURFACE ( 'NONE', #22374, 2.199999999999979750 ) ;
#20099 = ORIENTED_EDGE ( 'NONE', *, *, #6670, .T. ) ;
#20100 = CARTESIAN_POINT ( 'NONE',  ( 91.18044947428789726, 112.7436279071541776, -90.00000000000000000 ) ) ;
#20101 = DIRECTION ( 'NONE',  ( -1.000000000000000000, 0.000000000000000000, 0.000000000000000000 ) ) ;
#20102 = CARTESIAN_POINT ( 'NONE',  ( -281.7592670532760053, 269.1520027839447948, 145.8708543776411659 ) ) ;
#20103 = EDGE_CURVE ( 'NONE', #7964, #11181, #6141, .T. ) ;
#20104 = CARTESIAN_POINT ( 'NONE',  ( -20.63749999999999929, 0.000000000000000000, 0.000000000000000000 ) ) ;
#20105 = EDGE_CURVE ( 'NONE', #23533, #20130, #13109, .T. ) ;
#20106 = CARTESIAN_POINT ( 'NONE',  ( 0.000000000000000000, 0.000000000000000000, -8.499999999999998224 ) ) ;
#20107 = ORIENTED_EDGE ( 'NONE', *, *, #12125, .F. ) ;
#20108 = CARTESIAN_POINT ( 'NONE',  ( -24.83884780301426076, -996.7275481119216920, 145.0000119999999697 ) ) ;
#20109 = ORIENTED_EDGE ( 'NONE', *, *, #21647, .F. ) ;
#20110 = CARTESIAN_POINT ( 'NONE',  ( 0.000000000000000000, 0.000000000000000000, 90.00000000000000000 ) ) ;
#20111 = EDGE_LOOP ( 'NONE', ( #19011, #21268, #15434 ) ) ;
#20112 = DIRECTION ( 'NONE',  ( 0.000000000000000000, 0.000000000000000000, 1.000000000000000000 ) ) ;
#20113 = LINE ( 'NONE', #22272, #8809 ) ;
#20114 = DIRECTION ( 'NONE',  ( 0.000000000000000000, 0.000000000000000000, 1.000000000000000000 ) ) ;
#20115 = DIRECTION ( 'NONE',  ( 1.000000000000000000, 0.000000000000000000, 0.000000000000000000 ) ) ;
#20116 = FACE_BOUND ( 'NONE', #12628, .T. ) ;
#20117 = CARTESIAN_POINT ( 'NONE',  ( 4.154306624731137099, 2.398490048084935822, -3.721999068284414847 ) ) ;
#20118 = LINE ( 'NONE', #6981, #20165 ) ;
#20119 = VERTEX_POINT ( 'NONE', #3764 ) ;
#20120 = ORIENTED_EDGE ( 'NONE', *, *, #17902, .F. ) ;
#20121 = CARTESIAN_POINT ( 'NONE',  ( 0.000000000000000000, 0.000000000000000000, -5.000000000000000000 ) ) ;
#20122 = LINE ( 'NONE', #12576, #13154 ) ;
#20123 = ORIENTED_EDGE ( 'NONE', *, *, #8667, .F. ) ;
#20124 = EDGE_CURVE ( 'NONE', #5315, #11847, #5477, .T. ) ;
#20125 = LINE ( 'NONE', #11237, #3484 ) ;
#20126 = DIRECTION ( 'NONE',  ( -1.000000000000000000, 1.408839003528726857E-14, 6.982962677686266711E-15 ) ) ;
#20127 = ORIENTED_EDGE ( 'NONE', *, *, #3883, .F. ) ;
#20128 = CYLINDRICAL_SURFACE ( 'NONE', #2861, 24.99999999999998224 ) ;
#20129 = DIRECTION ( 'NONE',  ( -1.000000000000000000, 0.000000000000000000, 0.000000000000000000 ) ) ;
#20130 = VERTEX_POINT ( 'NONE', #5357 ) ;
#20131 = EDGE_CURVE ( 'NONE', #13840, #23140, #9296, .T. ) ;
#20132 = DIRECTION ( 'NONE',  ( 0.000000000000000000, -0.000000000000000000, 1.000000000000000000 ) ) ;
#20133 = LINE ( 'NONE', #13886, #8588 ) ;
#20134 = ORIENTED_EDGE ( 'NONE', *, *, #835, .F. ) ;
#20135 = EDGE_CURVE ( 'NONE', #5418, #4336, #8458, .T. ) ;
#20136 = DIRECTION ( 'NONE',  ( -1.000000000000000000, 1.408839003528726857E-14, 6.982962677686266711E-15 ) ) ;
#20137 = CARTESIAN_POINT ( 'NONE',  ( -158.1195828810603246, 116.4077317428680090, 27.50000000000675371 ) ) ;
#20138 = CARTESIAN_POINT ( 'NONE',  ( -7.894787914004607998, -1.230850257101226302E-13, -7.591390474663425536 ) ) ;
#20139 = VERTEX_POINT ( 'NONE', #14437 ) ;
#20140 = ORIENTED_EDGE ( 'NONE', *, *, #2157, .F. ) ;
#20141 = CARTESIAN_POINT ( 'NONE',  ( -5.000000000000000888, 6.123233995736767268E-16, 0.000000000000000000 ) ) ;
#20142 = AXIS2_PLACEMENT_3D ( 'NONE', #20766, #5920, #13450 ) ;
#20143 = PRODUCT_CONTEXT ( 'NONE', #8601, 'mechanical' ) ;
#20144 = FACE_OUTER_BOUND ( 'NONE', #7368, .T. ) ;
#20145 = CARTESIAN_POINT ( 'NONE',  ( -1.015826369459165157, 8.073766409993364590, -7.642786413619490737 ) ) ;
#20146 = CARTESIAN_POINT ( 'NONE',  ( 1.567478505476134606E-15, 4.618802153517012066, -3.433295621305382905 ) ) ;
#20147 = ORIENTED_EDGE ( 'NONE', *, *, #16202, .T. ) ;
#20148 = CARTESIAN_POINT ( 'NONE',  ( -23.72315261474503245, -8.055391459054616732, 145.0000119999999697 ) ) ;
#20149 = CIRCLE ( 'NONE', #109, 10.00000000000000000 ) ;
#20150 = APPLICATION_CONTEXT ( 'automotive_design' ) ;
#20151 = DIRECTION ( 'NONE',  ( 0.000000000000000000, -1.000000000000000000, -5.286776307738891306E-15 ) ) ;
#20152 = LINE ( 'NONE', #21738, #14924 ) ;
#20153 = ORIENTED_EDGE ( 'NONE', *, *, #10315, .F. ) ;
#20154 = CARTESIAN_POINT ( 'NONE',  ( -2.249192934210769784E-14, 9.016154170237596688, -7.999534413642735764 ) ) ;
#20155 = EDGE_CURVE ( 'NONE', #15468, #949, #5736, .T. ) ;
#20157 = EDGE_CURVE ( 'NONE', #10526, #20363, #10404, .T. ) ;
#20156 = ORIENTED_EDGE ( 'NONE', *, *, #6661, .F. ) ;
#20158 = CARTESIAN_POINT ( 'NONE',  ( 2.500000000000000888, 3.061616997868384127E-16, -4.974599999999998801 ) ) ;
#20159 = DIRECTION ( 'NONE',  ( -0.000000000000000000, -0.000000000000000000, 1.000000000000000000 ) ) ;
#20160 = ORIENTED_EDGE ( 'NONE', *, *, #60, .F. ) ;
#20161 = CARTESIAN_POINT ( 'NONE',  ( 1.312671235360372224, 3.860931062424219462, -0.05923475698270440348 ) ) ;
#20162 = DIRECTION ( 'NONE',  ( 1.000000000000000000, 0.000000000000000000, 0.000000000000000000 ) ) ;
#20163 = ADVANCED_FACE ( 'NONE', ( #20191 ), #16465, .F. ) ;
#20164 = DIRECTION ( 'NONE',  ( -0.7232617928448825673, 0.6905739489807055653, 6.982962677686266711E-15 ) ) ;
#20165 = VECTOR ( 'NONE', #12918, 999.9999999999998863 ) ;
#20166 = DIRECTION ( 'NONE',  ( 1.000000000000000000, 0.000000000000000000, 0.000000000000000000 ) ) ;
#20167 = PLANE ( 'NONE',  #3043 ) ;
#20168 = ORIENTED_EDGE ( 'NONE', *, *, #2070, .T. ) ;
#20169 = DIRECTION ( 'NONE',  ( 0.000000000000000000, 0.000000000000000000, -1.000000000000000000 ) ) ;
#20171 = EDGE_LOOP ( 'NONE', ( #20292, #12919, #15439, #7040 ) ) ;
#20170 = EDGE_LOOP ( 'NONE', ( #19518, #5823, #13733, #10317 ) ) ;
#20172 = DIRECTION ( 'NONE',  ( 0.000000000000000000, 0.000000000000000000, 1.000000000000000000 ) ) ;
#20173 = CARTESIAN_POINT ( 'NONE',  ( 0.000000000000000000, 0.000000000000000000, 3.469446951953614189E-15 ) ) ;
#20174 = CARTESIAN_POINT ( 'NONE',  ( 3.999999999999999112, 1.941961291383486277, -0.3515519931180248192 ) ) ;
#20175 = EDGE_LOOP ( 'NONE', ( #20515, #15918, #11104, #17439 ) ) ;
#20176 = FACE_OUTER_BOUND ( 'NONE', #15586, .T. ) ;
#20177 = VECTOR ( 'NONE', #10703, 1000.000000000000000 ) ;
#20178 = LINE ( 'NONE', #23688, #3741 ) ;
#20179 = ORIENTED_EDGE ( 'NONE', *, *, #20310, .F. ) ;
#20180 = EDGE_CURVE ( 'NONE', #13071, #6769, #15030, .T. ) ;
#20181 = ADVANCED_FACE ( 'NONE', ( #8008 ), #15150, .T. ) ;
#20182 = DIRECTION ( 'NONE',  ( 0.000000000000000000, 0.000000000000000000, -1.000000000000000000 ) ) ;
#20183 = DIRECTION ( 'NONE',  ( 0.000000000000000000, 0.000000000000000000, 1.000000000000000000 ) ) ;
#20184 = EDGE_LOOP ( 'NONE', ( #8947, #17427, #19537, #13488, #9101, #6654 ) ) ;
#20185 = ORIENTED_EDGE ( 'NONE', *, *, #1350, .F. ) ;
#20186 = DIRECTION ( 'NONE',  ( 1.000000000000000000, -3.495664435217746987E-15, -0.000000000000000000 ) ) ;
#20187 = ORIENTED_EDGE ( 'NONE', *, *, #16363, .T. ) ;
#20188 =( REPRESENTATION_RELATIONSHIP ('NONE','NONE', #10127, #22995 ) REPRESENTATION_RELATIONSHIP_WITH_TRANSFORMATION ( #12525 )SHAPE_REPRESENTATION_RELATIONSHIP( ) );
#20189 = CARTESIAN_POINT ( 'NONE',  ( 21.69904058241862543, -987.4760093562550765, -145.0000000000001421 ) ) ;
#20190 = EDGE_CURVE ( 'NONE', #5401, #9508, #287, .T. ) ;
#20191 = FACE_OUTER_BOUND ( 'NONE', #21007, .T. ) ;
#20192 = LINE ( 'NONE', #7280, #692 ) ;
#20193=STYLED_ITEM('',(#23934),#11885);
#20194 = PRODUCT ( 'socket head cap screw_iso_ISO 4762 M5 x 16 - 16N', 'socket head cap screw_iso_ISO 4762 M5 x 16 - 16N', '', ( #7357 ) ) ;
#20195 = CIRCLE ( 'NONE', #10589, 2.055000000000001492 ) ;
#20196 = CARTESIAN_POINT ( 'NONE',  ( -52.99999999999997158, -56.80000000000005400, 2.098186183925023932E-13 ) ) ;
#20197 = PLANE ( 'NONE',  #10807 ) ;
#20198 = SHAPE_REPRESENTATION_RELATIONSHIP ( 'NONE' , 'NONE' ,  #8847, #11926 ) ;
#20199 = ORIENTED_EDGE ( 'NONE', *, *, #787, .F. ) ;
#20200 = EDGE_CURVE ( 'NONE', #1157, #12819, #11535, .T. ) ;
#20201 = SURFACE_STYLE_USAGE ( .BOTH. , #7776 ) ;
#20202 = DIRECTION ( 'NONE',  ( -1.000000000000000000, 0.000000000000000000, 0.000000000000000000 ) ) ;
#20203 = CARTESIAN_POINT ( 'NONE',  ( -0.5469614295416921346, 4.303013824936271270, -3.535263753543735454 ) ) ;
#20204 = ORIENTED_EDGE ( 'NONE', *, *, #9417, .T. ) ;
#20205 = CARTESIAN_POINT ( 'NONE',  ( 280.0627656775836272, 270.0000000000000000, -145.1452901038202015 ) ) ;
#20206 = DIRECTION ( 'NONE',  ( 0.000000000000000000, 0.000000000000000000, 1.000000000000000000 ) ) ;
#20207 = DIRECTION ( 'NONE',  ( 1.000000000000000000, 0.000000000000000000, 0.000000000000000000 ) ) ;
#20208 = VECTOR ( 'NONE', #22149, 1000.000000000000000 ) ;
#20209 = TOROIDAL_SURFACE ( 'NONE', #6333, 4.000000000000000000, 0.2500000000000000000 ) ;
#20210 = CARTESIAN_POINT ( 'NONE',  ( 45.00000000000000000, 272.9999999999999432, 0.000000000000000000 ) ) ;
#20211 = CARTESIAN_POINT ( 'NONE',  ( -100.0000000000001137, -132.1999999999992212, 147.2000000000013813 ) ) ;
#20212 = ORIENTED_EDGE ( 'NONE', *, *, #9316, .T. ) ;
#20213 = CARTESIAN_POINT ( 'NONE',  ( -16.52066876451829458, -981.1653297051910840, 145.0000119999999697 ) ) ;
#20214 = ORIENTED_EDGE ( 'NONE', *, *, #17022, .T. ) ;
#20215 = AXIS2_PLACEMENT_3D ( 'NONE', #8476, #10548, #21498 ) ;
#20216 = DIRECTION ( 'NONE',  ( -0.000000000000000000, -0.000000000000000000, 1.000000000000000000 ) ) ;
#20217 = CARTESIAN_POINT ( 'NONE',  ( -79.99999999999995737, -138.0000000000000284, 0.000000000000000000 ) ) ;
#20218 = EDGE_CURVE ( 'NONE', #13773, #9902, #9638, .T. ) ;
#20219 = ORIENTED_EDGE ( 'NONE', *, *, #14712, .T. ) ;
#20220 =( NAMED_UNIT ( * ) SI_UNIT ( $, .STERADIAN. ) SOLID_ANGLE_UNIT ( ) );
#20221 = CARTESIAN_POINT ( 'NONE',  ( 2.500000000000002220, 2.357898499370434386, -3.469446951953614189E-15 ) ) ;
#20222 = EDGE_CURVE ( 'NONE', #7277, #8336, #4263, .T. ) ;
#20223 = CARTESIAN_POINT ( 'NONE',  ( 1.500000000000001332, 9.797174393178825657E-16, -8.000000000000000000 ) ) ;
#20224 = FACE_OUTER_BOUND ( 'NONE', #6710, .T. ) ;
#20225 = EDGE_CURVE ( 'NONE', #21875, #1621, #14722, .T. ) ;
#20226 = DIRECTION ( 'NONE',  ( -0.8660254037844382635, -0.5000000000000004441, 0.000000000000000000 ) ) ;
#20227 = CARTESIAN_POINT ( 'NONE',  ( -145.0000000000000284, -1000.000000000000000, 90.00000000000000000 ) ) ;
#20228 = CARTESIAN_POINT ( 'NONE',  ( 24.83884780301427142, 3.272451888078352855, 145.0000119999999981 ) ) ;
#20229 = ORIENTED_EDGE ( 'NONE', *, *, #22341, .T. ) ;
#20230 = EDGE_CURVE ( 'NONE', #5086, #19875, #14909, .T. ) ;
#20231 = VERTEX_POINT ( 'NONE', #17185 ) ;
#20232 = DIRECTION ( 'NONE',  ( 0.000000000000000000, 0.000000000000000000, -1.000000000000000000 ) ) ;
#20233 = CARTESIAN_POINT ( 'NONE',  ( 0.000000000000000000, -2.342598717236900718, 4.057500000000001883 ) ) ;
#20234 = EDGE_CURVE ( 'NONE', #3110, #22784, #4000, .T. ) ;
#20235 = VERTEX_POINT ( 'NONE', #22240 ) ;
#20236 = TOROIDAL_SURFACE ( 'NONE', #14478, 5.400000000000002132, 0.4000000000000000222 ) ;
#20237 = VECTOR ( 'NONE', #1791, 1000.000000000000000 ) ;
#20238 = DIRECTION ( 'NONE',  ( 1.000000000000000000, 0.000000000000000000, -0.000000000000000000 ) ) ;
#20239 = CARTESIAN_POINT ( 'NONE',  ( 4.406466114817131796, -6.116179640279303165, -7.446478553994418270 ) ) ;
#20240 = ORIENTED_EDGE ( 'NONE', *, *, #18278, .F. ) ;
#20241 = DIRECTION ( 'NONE',  ( 1.000000000000000000, 0.000000000000000000, 0.000000000000000000 ) ) ;
#20242 = CARTESIAN_POINT ( 'NONE',  ( -9.999999999999998224, -6.123233995736763324E-16, 200.0000060000000133 ) ) ;
#20243 = EDGE_LOOP ( 'NONE', ( #16981, #23403, #2074, #7310, #23174, #7947, #11361, #8100 ) ) ;
#20244 = CIRCLE ( 'NONE', #9866, 5.199999999999982414 ) ;
#20245 = DIRECTION ( 'NONE',  ( 1.224646799147353207E-16, 1.000000000000000000, 0.000000000000000000 ) ) ;
#20246 = LINE ( 'NONE', #7450, #15533 ) ;
#20247 = CARTESIAN_POINT ( 'NONE',  ( -10.00000000000000178, -1.308996938995748760, 200.0000120000000550 ) ) ;
#20248 = ORIENTED_EDGE ( 'NONE', *, *, #23141, .F. ) ;
#20249 = DIRECTION ( 'NONE',  ( -1.000000000000000000, -2.775557561562891351E-17, -0.000000000000000000 ) ) ;
#20250 = CARTESIAN_POINT ( 'NONE',  ( -136.3934655611483322, -1073.633154336009738, 27.82653936295263719 ) ) ;
#20251 = ORIENTED_EDGE ( 'NONE', *, *, #13547, .F. ) ;
#20252 = VERTEX_POINT ( 'NONE', #638 ) ;
#20253 = FACE_OUTER_BOUND ( 'NONE', #239, .T. ) ;
#20254 = CIRCLE ( 'NONE', #17943, 2.649999999999999467 ) ;
#20255 = DIRECTION ( 'NONE',  ( 1.000000000000000000, 0.000000000000000000, 0.000000000000000000 ) ) ;
#20256 = LINE ( 'NONE', #9306, #18452 ) ;
#20257 = DIRECTION ( 'NONE',  ( -1.110223024625155594E-14, 0.000000000000000000, -1.000000000000000000 ) ) ;
#20258 = VERTEX_POINT ( 'NONE', #22726 ) ;
#20259 = EDGE_CURVE ( 'NONE', #4691, #13380, #20917, .T. ) ;
#20260 = DIRECTION ( 'NONE',  ( 0.000000000000000000, 1.224646799147357891E-16, 1.000000000000000000 ) ) ;
#20261 = AXIS2_PLACEMENT_3D ( 'NONE', #1278, #1032, #2745 ) ;
#20262 = EDGE_CURVE ( 'NONE', #2548, #13805, #11419, .T. ) ;
#20263 = CIRCLE ( 'NONE', #21429, 5.249999999999973355 ) ;
#20264 = UNCERTAINTY_MEASURE_WITH_UNIT (LENGTH_MEASURE( 1.000000000000000082E-05 ), #18227, 'distance_accuracy_value', 'NONE');
#20265 = CIRCLE ( 'NONE', #21812, 35.00000000000000711 ) ;
#20266 = DIRECTION ( 'NONE',  ( 0.000000000000000000, 0.000000000000000000, -1.000000000000000000 ) ) ;
#20267 = LINE ( 'NONE', #9186, #5296 ) ;
#20268 = VERTEX_POINT ( 'NONE', #7515 ) ;
#20269 = DIRECTION ( 'NONE',  ( 0.000000000000000000, -1.000000000000000000, 3.469446951953614189E-15 ) ) ;
#20270 = ORIENTED_EDGE ( 'NONE', *, *, #14501, .F. ) ;
#20271 = CIRCLE ( 'NONE', #13385, 2.649999999999985700 ) ;
#20272 = DIRECTION ( 'NONE',  ( 0.000000000000000000, 1.000000000000000000, -1.287488025362403787E-15 ) ) ;
#20273 = CARTESIAN_POINT ( 'NONE',  ( 57.99999999999999289, 0.000000000000000000, 0.000000000000000000 ) ) ;
#20274 = VERTEX_POINT ( 'NONE', #20440 ) ;
#20275 = DIRECTION ( 'NONE',  ( 0.000000000000000000, 0.000000000000000000, 1.000000000000000000 ) ) ;
#20276 = CARTESIAN_POINT ( 'NONE',  ( -79.99999999999995737, -62.00000000000004263, 3.000000000000000000 ) ) ;
#20277 = CARTESIAN_POINT ( 'NONE',  ( 6.482064212728083419, -1024.200416217147222, 145.0000119999999697 ) ) ;
#20278 = CARTESIAN_POINT ( 'NONE',  ( 280.3431883596740590, 272.9999999999998295, 145.0627246250092242 ) ) ;
#20279 = MANIFOLD_SOLID_BREP ( 'OuterRace', #12214 ) ;
#20280 = CARTESIAN_POINT ( 'NONE',  ( 125.2206635291104249, -1091.349901830162707, -32.17188107257626939 ) ) ;
#20281 = CARTESIAN_POINT ( 'NONE',  ( -20.00000000000000000, 2.449293598294706513E-15, 138.9999999999999716 ) ) ;
#20282 = ORIENTED_EDGE ( 'NONE', *, *, #12859, .F. ) ;
#20283 = DIRECTION ( 'NONE',  ( 0.000000000000000000, 1.000000000000000000, -1.224646799147353207E-16 ) ) ;
#20284 = FACE_OUTER_BOUND ( 'NONE', #3371, .T. ) ;
#20285 = PRODUCT_DEFINITION_SHAPE ( 'NONE', 'NONE',  #23889 ) ;
#20287 = ORIENTED_EDGE ( 'NONE', *, *, #8188, .F. ) ;
#20286 = ORIENTED_EDGE ( 'NONE', *, *, #21494, .F. ) ;
#20288 = DIRECTION ( 'NONE',  ( 1.224646799147353207E-16, -4.064521778635712183E-50, -1.000000000000000000 ) ) ;
#20289 = CARTESIAN_POINT ( 'NONE',  ( -144.8060344827586050, -7.497491405672224829, -90.00000000000000000 ) ) ;
#20290 = CIRCLE ( 'NONE', #1783, 2.649999999999999467 ) ;
#20291 = LINE ( 'NONE', #2055, #15363 ) ;
#20292 = ORIENTED_EDGE ( 'NONE', *, *, #16200, .F. ) ;
#20293 = DIRECTION ( 'NONE',  ( 1.000000000000000000, -6.640089860198304064E-16, -0.000000000000000000 ) ) ;
#20294 = VERTEX_POINT ( 'NONE', #3896 ) ;
#20295 = CARTESIAN_POINT ( 'NONE',  ( -45.00000000000000000, 269.9999999999999432, 0.000000000000000000 ) ) ;
#20296 = ORIENTED_EDGE ( 'NONE', *, *, #22469, .F. ) ;
#20297 = DIRECTION ( 'NONE',  ( 0.000000000000000000, 0.000000000000000000, -1.000000000000000000 ) ) ;
#20298 = VECTOR ( 'NONE', #2049, 1000.000000000000000 ) ;
#20299 = ORIENTED_EDGE ( 'NONE', *, *, #19162, .T. ) ;
#20300 = CARTESIAN_POINT ( 'NONE',  ( 124.5680376182010320, -1092.237904323006205, 32.50000000000647304 ) ) ;
#20301 = ORIENTED_EDGE ( 'NONE', *, *, #12724, .F. ) ;
#20302 = CONICAL_SURFACE ( 'NONE', #4122, 2.055000000000000160, 0.7853981633974717047 ) ;
#20303 = CARTESIAN_POINT ( 'NONE',  ( -280.0000000000000568, 272.9999999999999432, 145.0000000000000284 ) ) ;
#20304 = DIRECTION ( 'NONE',  ( 0.000000000000000000, 0.000000000000000000, 1.000000000000000000 ) ) ;
#20305 = CARTESIAN_POINT ( 'NONE',  ( -79.04925354955248906, 121.5574576620396812, -2.775557561562891351E-14 ) ) ;
#20306 = DIRECTION ( 'NONE',  ( 0.000000000000000000, 0.000000000000000000, -1.000000000000000000 ) ) ;
#20307 = DIRECTION ( 'NONE',  ( 1.000000000000000000, -0.000000000000000000, -0.000000000000000000 ) ) ;
#20308 = DIRECTION ( 'NONE',  ( 1.000000000000000000, 0.000000000000000000, 0.000000000000000000 ) ) ;
#20309 = EDGE_LOOP ( 'NONE', ( #4792, #2453, #21025, #21446 ) ) ;
#20310 = EDGE_CURVE ( 'NONE', #590, #23044, #13130, .T. ) ;
#20311 = CARTESIAN_POINT ( 'NONE',  ( 5.200000000000002842, 3.061616997868383634E-16, -2.500000000000000444 ) ) ;
#20312 = DIRECTION ( 'NONE',  ( 1.000000000000000000, 0.000000000000000000, 0.000000000000000000 ) ) ;
#20313 = EDGE_CURVE ( 'NONE', #23227, #23365, #3003, .T. ) ;
#20314 = EDGE_CURVE ( 'NONE', #12183, #733, #12323, .T. ) ;
#20315 = VECTOR ( 'NONE', #11626, 1000.000000000000000 ) ;
#20316 = APPLICATION_CONTEXT ( 'automotive_design' ) ;
#20317 = ORIENTED_EDGE ( 'NONE', *, *, #1554, .F. ) ;
#20318 = DIRECTION ( 'NONE',  ( -1.000000000000000000, -2.775557561562891351E-17, 0.000000000000000000 ) ) ;
#20319 = DIRECTION ( 'NONE',  ( 1.000000000000000000, -0.000000000000000000, -0.000000000000000000 ) ) ;
#20320 = AXIS2_PLACEMENT_3D ( 'NONE', #5032, #16512, #12827 ) ;
#20321 = EDGE_CURVE ( 'NONE', #16807, #9811, #23637, .T. ) ;
#20322 = AXIS2_PLACEMENT_3D ( 'NONE', #10681, #11035, #7028 ) ;
#20323 = CARTESIAN_POINT ( 'NONE',  ( 7.500000000000000888, 2.932633423934449812, -0.4709827563909316783 ) ) ;
#20324 = DIRECTION ( 'NONE',  ( 0.9289202219288174023, 0.3702799228849934510, 6.982962677686266711E-15 ) ) ;
#20325 = CARTESIAN_POINT ( 'NONE',  ( 280.9955614683501608, 270.4045710003932754, -149.5135885331258692 ) ) ;
#20326 = ORIENTED_EDGE ( 'NONE', *, *, #15822, .T. ) ;
#20327 = CARTESIAN_POINT ( 'NONE',  ( 0.2500000000000002220, 0.000000000000000000, 0.000000000000000000 ) ) ;
#20328 = VERTEX_POINT ( 'NONE', #6306 ) ;
#20329 = CARTESIAN_POINT ( 'NONE',  ( 4.999999999999997335, 0.000000000000000000, 0.000000000000000000 ) ) ;
#20330 = CARTESIAN_POINT ( 'NONE',  ( -20.63749999999999929, 2.632990618166809235E-15, 21.50000000000000000 ) ) ;
#20331 = CARTESIAN_POINT ( 'NONE',  ( -175.1609685624542294, -1088.719770019218458, -27.49999999999322498 ) ) ;
#20332 = ORIENTED_EDGE ( 'NONE', *, *, #9042, .F. ) ;
#20333 = AXIS2_PLACEMENT_3D ( 'NONE', #1619, #17934, #12656 ) ;
#20334 = CARTESIAN_POINT ( 'NONE',  ( 123.3268328482423044, -1093.890927824661958, -28.34359615383078790 ) ) ;
#20335 = FACE_OUTER_BOUND ( 'NONE', #6140, .T. ) ;
#20336 = CARTESIAN_POINT ( 'NONE',  ( 91.18044947429038416, -112.7436279071521881, -90.00000000000000000 ) ) ;
#20338 = AXIS2_PLACEMENT_3D ( 'NONE', #1707, #13470, #9569 ) ;
#20337 = CARTESIAN_POINT ( 'NONE',  ( -7.808218555861951238, 4.508077085120201666, -7.999534413642737540 ) ) ;
#20339 = DIRECTION ( 'NONE',  ( 1.000000000000000000, 0.000000000000000000, 0.000000000000000000 ) ) ;
#20340 = CIRCLE ( 'NONE', #11529, 5.249999999999991118 ) ;
#20341 = CARTESIAN_POINT ( 'NONE',  ( 282.1999999999999318, 269.9999999999999432, 146.4928932188134638 ) ) ;
#20342 = VECTOR ( 'NONE', #4360, 1000.000000000000114 ) ;
#20343 = EDGE_LOOP ( 'NONE', ( #10992, #13696, #1501, #17372, #892, #15503, #13280, #6988, #14690, #789, #22413, #21248 ) ) ;
#20344 = VERTEX_POINT ( 'NONE', #17785 ) ;
#20345 = DIRECTION ( 'NONE',  ( 1.110223024625155594E-14, 0.000000000000000000, -1.000000000000000000 ) ) ;
#20346 = CYLINDRICAL_SURFACE ( 'NONE', #6166, 5.249999999999942268 ) ;
#20347 = ORIENTED_EDGE ( 'NONE', *, *, #6630, .F. ) ;
#20348 = EDGE_CURVE ( 'NONE', #7964, #22508, #2559, .T. ) ;
#20349 = CARTESIAN_POINT ( 'NONE',  ( 45.00000000000002132, -52.79999999999934346, 195.0000000000002274 ) ) ;
#20350 = CARTESIAN_POINT ( 'NONE',  ( 7.848314987057850800, -4.129027267381569999, -7.493854785173811095 ) ) ;
#20351 = ADVANCED_FACE ( 'NONE', ( #1227 ), #11905, .F. ) ;
#20352 = CARTESIAN_POINT ( 'NONE',  ( 280.5743436287469308, 269.9433523009093392, -145.2481149223241061 ) ) ;
#20353 = ADVANCED_FACE ( 'NONE', ( #17643 ), #12142, .F. ) ;
#20354 = ORIENTED_EDGE ( 'NONE', *, *, #15638, .T. ) ;
#20355 = AXIS2_PLACEMENT_3D ( 'NONE', #2689, #21036, #8599 ) ;
#20356 = VECTOR ( 'NONE', #18916, 1000.000000000000114 ) ;
#20357 = CARTESIAN_POINT ( 'NONE',  ( 0.2500000000000002220, 0.000000000000000000, 0.000000000000000000 ) ) ;
#20358 = CARTESIAN_POINT ( 'NONE',  ( 126.3653543294818178, 77.28387428943173632, -29.99999999999356604 ) ) ;
#20359 = AXIS2_PLACEMENT_3D ( 'NONE', #20800, #8334, #18730 ) ;
#20360 = VECTOR ( 'NONE', #14108, 1000.000000000000000 ) ;
#20361 = EDGE_CURVE ( 'NONE', #19693, #14422, #4551, .T. ) ;
#20362 = CARTESIAN_POINT ( 'NONE',  ( 0.000000000000000000, -131.7994082814339833, 3.000000000000000000 ) ) ;
#20363 = VERTEX_POINT ( 'NONE', #17425 ) ;
#20364 = CARTESIAN_POINT ( 'NONE',  ( 7.500000000000000000, 4.330127018922190096, -7.422398894150032511 ) ) ;
#20366 = CARTESIAN_POINT ( 'NONE',  ( 35.00000000000000000, 4.286263797015736496E-15, 100.0000000000000000 ) ) ;
#20365 = PRODUCT_DEFINITION ( 'UNKNOWN', '', #6575, #14862 ) ;
#20367 = EDGE_LOOP ( 'NONE', ( #22860, #7141 ) ) ;
#20368 = LINE ( 'NONE', #13063, #1904 ) ;
#20369 = APPLICATION_PROTOCOL_DEFINITION ( 'draft international standard', 'automotive_design', 1998, #9845 ) ;
#20370 = B_SPLINE_CURVE_WITH_KNOTS ( 'NONE', 3,
 ( #7942, #22535, #11843, #15204, #20601, #11721 ),
 .UNSPECIFIED., .F., .F.,
 ( 4, 2, 4 ),
 ( 0.002452478801916361129, 0.003676905084148001344, 0.004901331366379641126 ),
 .UNSPECIFIED. ) ;
#20371 = DIRECTION ( 'NONE',  ( 1.000000000000000000, 0.000000000000000000, 0.000000000000000000 ) ) ;
#20372 = DIRECTION ( 'NONE',  ( -1.000000000000000000, 1.408839003528726857E-14, 6.982962677686266711E-15 ) ) ;
#20373 = CARTESIAN_POINT ( 'NONE',  ( 4.000000000000000000, 2.309401076758497151, -3.433295621305379353 ) ) ;
#20374 = EDGE_LOOP ( 'NONE', ( #11337, #20229, #12872, #19292, #13909, #15104, #7740, #3681 ) ) ;
#20375 = VECTOR ( 'NONE', #1490, 1000.000000000000000 ) ;
#20376 = ORIENTED_EDGE ( 'NONE', *, *, #5335, .F. ) ;
#20377 = AXIS2_PLACEMENT_3D ( 'NONE', #11225, #8924, #23624 ) ;
#20378 = AXIS2_PLACEMENT_3D ( 'NONE', #13535, #17232, #14226 ) ;
#20379 = CARTESIAN_POINT ( 'NONE',  ( 140.0355749532213565, -37.61698748598472974, -2.775557561562891351E-14 ) ) ;
#20380 = VECTOR ( 'NONE', #9774, 1000.000000000000000 ) ;
#20381 = AXIS2_PLACEMENT_3D ( 'NONE', #6199, #22841, #6307 ) ;
#20382 = AXIS2_PLACEMENT_3D ( 'NONE', #19711, #4640, #8868 ) ;
#20383 = EDGE_LOOP ( 'NONE', ( #5458, #7811, #6116, #7639 ) ) ;
#20384 = CARTESIAN_POINT ( 'NONE',  ( 2.000000000000008882, 3.464101615137749945, 0.000000000000000000 ) ) ;
#20385 = DIRECTION ( 'NONE',  ( -0.5000000000000051070, 0.000000000000000000, 0.8660254037844355990 ) ) ;
#20386 = ORIENTED_EDGE ( 'NONE', *, *, #13051, .T. ) ;
#20387 = DIRECTION ( 'NONE',  ( 1.000000000000000000, 0.000000000000000000, 0.000000000000000000 ) ) ;
#20388 = ORIENTED_EDGE ( 'NONE', *, *, #16574, .F. ) ;
#20389 = CIRCLE ( 'NONE', #13512, 2.499999999999998668 ) ;
#20390 = CIRCLE ( 'NONE', #13131, 7.500000000000000888 ) ;
#20391 = EDGE_CURVE ( 'NONE', #4114, #23301, #9572, .T. ) ;
#20392 = EDGE_CURVE ( 'NONE', #16958, #9995, #1842, .T. ) ;
#20394 = AXIS2_PLACEMENT_3D ( 'NONE', #1616, #9356, #22021 ) ;
#20393 = COLOUR_RGB ( '',1.000000000000000000, 0.9490196078431372140, 0.9098039215686274384 ) ;
#20396 = DIRECTION ( 'NONE',  ( 0.000000000000000000, 0.000000000000000000, -1.000000000000000000 ) ) ;
#20395 = CIRCLE ( 'NONE', #16617, 145.0000000000000284 ) ;
#20397 = ADVANCED_FACE ( 'NONE', ( #15866 ), #9951, .T. ) ;
#20399 = VECTOR ( 'NONE', #13448, 1000.000000000000000 ) ;
#20398 = DIRECTION ( 'NONE',  ( 0.000000000000000000, 1.000000000000000000, -1.287488025362403787E-15 ) ) ;
#20400 = EDGE_LOOP ( 'NONE', ( #14449, #17888 ) ) ;
#20401 = LINE ( 'NONE', #14873, #23521 ) ;
#20402 = VECTOR ( 'NONE', #11718, 1000.000000000000000 ) ;
#20403 = B_SPLINE_CURVE_WITH_KNOTS ( 'NONE', 3,
 ( #5251, #9246, #14344, #18054, #21675, #7056, #14799, #5132, #12543 ),
 .UNSPECIFIED., .F., .F.,
 ( 4, 2, 1, 2, 4 ),
 ( 0.000000000000000000, 0.002165063509461097498, 0.004330127018922194995, 0.006495190528383292493, 0.008660254037844389990 ),
 .UNSPECIFIED. ) ;
#20404 = DIRECTION ( 'NONE',  ( -1.000000000000000000, -0.000000000000000000, -0.000000000000000000 ) ) ;
#20405 = CARTESIAN_POINT ( 'NONE',  ( 279.9999999999999432, 272.9999999999999432, 145.0000000000000284 ) ) ;
#20406 = CARTESIAN_POINT ( 'NONE',  ( 0.000000000000000000, 0.000000000000000000, -150.0000000000000000 ) ) ;
#20407 = DIRECTION ( 'NONE',  ( -0.7071067811865369146, 0.000000000000000000, 0.7071067811865582309 ) ) ;
#20408 = ORIENTED_EDGE ( 'NONE', *, *, #4437, .F. ) ;
#20409 = CARTESIAN_POINT ( 'NONE',  ( 65.00000000000005684, -52.79999999999970584, 35.00000000000017764 ) ) ;
#20410 = FACE_OUTER_BOUND ( 'NONE', #15391, .T. ) ;
#20411 =( NAMED_UNIT ( * ) SI_UNIT ( $, .STERADIAN. ) SOLID_ANGLE_UNIT ( ) );
#20412 = B_SPLINE_CURVE_WITH_KNOTS ( 'NONE', 3,
 ( #21950, #1774, #221, #22064, #5531, #3018, #20250, #9164, #22178, #2012, #10434, #3700, #17779, #11117, #2732, #5422, #1223, #9402, #8594, #5295, #7575, #15966, #16523, #11001, #12833, #18437, #23310, #3481, #6778, #21501, #10891, #9047 ),
 .UNSPECIFIED., .F., .F.,
 ( 4, 2, 2, 2, 2, 2, 2, 2, 2, 2, 2, 2, 2, 2, 2, 4 ),
 ( 2.964296775167216948E-17, 0.0004914281572964689527, 0.0009828563145929084151, 0.001474284471889347877, 0.001965712629185786906, 0.002457140786482226585, 0.002948568943778665831, 0.003931425258371301461, 0.004422853415667624480, 0.004914281572963947499, 0.005405709730260270518, 0.005897137887556594404, 0.006388566044852917424, 0.006879994202149240443, 0.007371422359445564329, 0.007862850516741886481 ),
 .UNSPECIFIED. ) ;
#20414 = VERTEX_POINT ( 'NONE', #10184 ) ;
#20413 = ORIENTED_EDGE ( 'NONE', *, *, #4638, .T. ) ;
#20415 = DIRECTION ( 'NONE',  ( 0.000000000000000000, 0.000000000000000000, 1.000000000000000000 ) ) ;
#20417 = AXIS2_PLACEMENT_3D ( 'NONE', #15892, #23225, #19122 ) ;
#20416 = AXIS2_PLACEMENT_3D ( 'NONE', #13491, #2702, #4384 ) ;
#20418 = CARTESIAN_POINT ( 'NONE',  ( -136.8702482660837347, -1072.742966597997338, -31.11320915316586522 ) ) ;
#20419 = CARTESIAN_POINT ( 'NONE',  ( 0.000000000000000000, 0.000000000000000000, -0.3080913168122742518 ) ) ;
#20420 =( GEOMETRIC_REPRESENTATION_CONTEXT ( 3 ) GLOBAL_UNCERTAINTY_ASSIGNED_CONTEXT ( ( #17422 ) ) GLOBAL_UNIT_ASSIGNED_CONTEXT ( ( #16356, #10948, #19143 ) ) REPRESENTATION_CONTEXT ( 'NONE', 'WORKASPACE' ) );
#20421 = AXIS2_PLACEMENT_3D ( 'NONE', #5959, #15985, #4865 ) ;
#20422 = VECTOR ( 'NONE', #610, 1000.000000000000000 ) ;
#20423 = VECTOR ( 'NONE', #10261, 1000.000000000000000 ) ;
#20424 = ORIENTED_EDGE ( 'NONE', *, *, #12364, .T. ) ;
#20425 = DIRECTION ( 'NONE',  ( 0.000000000000000000, -2.618450529776313049E-15, -1.000000000000000000 ) ) ;
#20426 = EDGE_LOOP ( 'NONE', ( #13568, #3862, #276, #5794 ) ) ;
#20427 = CARTESIAN_POINT ( 'NONE',  ( 285.1999999999999886, 268.1431883596741841, -146.4301685938041828 ) ) ;
#20428 = ORIENTED_EDGE ( 'NONE', *, *, #6767, .F. ) ;
#20429 = ADVANCED_FACE ( 'NONE', ( #8140 ), #17527, .T. ) ;
#20430 = DIRECTION ( 'NONE',  ( 1.350636282998972974E-14, 0.000000000000000000, -1.000000000000000000 ) ) ;
#20431 = CARTESIAN_POINT ( 'NONE',  ( 24.99999999999998579, 45.00100000000075084, 154.9999999999998579 ) ) ;
#20432 = ITEM_DEFINED_TRANSFORMATION ( 'NONE', 'NONE', #16594,  #11210 ) ;
#20433 = VERTEX_POINT ( 'NONE', #15735 ) ;
#20434 = ADVANCED_FACE ( 'NONE', ( #21641 ), #7247, .F. ) ;
#20435 = FACE_OUTER_BOUND ( 'NONE', #19794, .T. ) ;
#20436 = AXIS2_PLACEMENT_3D ( 'NONE', #7004, #19788, #21728 ) ;
#20437 = ORIENTED_EDGE ( 'NONE', *, *, #1075, .T. ) ;
#20438 = CARTESIAN_POINT ( 'NONE',  ( -128.9672686250725633, 85.97940096925731268, 31.66065886938990914 ) ) ;
#20439 = VECTOR ( 'NONE', #3114, 1000.000000000000000 ) ;
#20440 = CARTESIAN_POINT ( 'NONE',  ( -121.5574576620394112, -79.04925354955290118, -90.00000000000000000 ) ) ;
#20441 = AXIS2_PLACEMENT_3D ( 'NONE', #23150, #11978, #21100 ) ;
#20442 = CIRCLE ( 'NONE', #16978, 2.649999999999985700 ) ;
#20443 = FACE_OUTER_BOUND ( 'NONE', #6720, .T. ) ;
#20444 = DIRECTION ( 'NONE',  ( 0.000000000000000000, 0.000000000000000000, 1.000000000000000000 ) ) ;
#20445 = CARTESIAN_POINT ( 'NONE',  ( -281.6574776399289703, 269.2538215477172230, 145.8086578304521197 ) ) ;
#20446 = CARTESIAN_POINT ( 'NONE',  ( 5.200000000000002842, 0.000000000000000000, 0.000000000000000000 ) ) ;
#20447 = ORIENTED_EDGE ( 'NONE', *, *, #19391, .T. ) ;
#20448 = CARTESIAN_POINT ( 'NONE',  ( 0.000000000000000000, 0.000000000000000000, 0.000000000000000000 ) ) ;
#20449 = CARTESIAN_POINT ( 'NONE',  ( 2.500000000000000000, 0.000000000000000000, 0.000000000000000000 ) ) ;
#20450 = CARTESIAN_POINT ( 'NONE',  ( 131.6528213848855273, 81.80793830425525925, -31.11299551804357932 ) ) ;
#20451 = CARTESIAN_POINT ( 'NONE',  ( 279.9999999999999432, 273.0299999999999159, 145.0000000000000284 ) ) ;
#20452 = DIRECTION ( 'NONE',  ( 0.000000000000000000, -1.000000000000000000, -1.110223024625156540E-16 ) ) ;
#20453 = CARTESIAN_POINT ( 'NONE',  ( 133.9969223633119384, 77.90910650221383094, 31.11216498479350179 ) ) ;
#20454 = EDGE_CURVE ( 'NONE', #10981, #2765, #6479, .T. ) ;
#20455 = ADVANCED_FACE ( 'NONE', ( #5450 ), #8724, .F. ) ;
#20456 = DIRECTION ( 'NONE',  ( -1.000000000000000000, -2.775557561562891351E-17, 0.000000000000000000 ) ) ;
#20457 = CARTESIAN_POINT ( 'NONE',  ( -281.3518577254347406, 272.8327955282141488, -145.2494876630256613 ) ) ;
#20458 = CONTEXT_DEPENDENT_SHAPE_REPRESENTATION ( #18767, #21646 ) ;
#20459 = EDGE_LOOP ( 'NONE', ( #2260, #18415, #20751, #18860 ) ) ;
#20460 = CARTESIAN_POINT ( 'NONE',  ( -21.69578997558839006, -987.4712331462251313, 145.0000119999999697 ) ) ;
#20461 = ORIENTED_EDGE ( 'NONE', *, *, #8482, .F. ) ;
#20462 = FACE_OUTER_BOUND ( 'NONE', #4153, .T. ) ;
#20463 = DIRECTION ( 'NONE',  ( 1.000000000000000000, -0.000000000000000000, -0.000000000000000000 ) ) ;
#20464 = FACE_OUTER_BOUND ( 'NONE', #3028, .T. ) ;
#20465 = EDGE_CURVE ( 'NONE', #19969, #21767, #14641, .T. ) ;
#20466 = EDGE_LOOP ( 'NONE', ( #13479, #5164, #8401, #12188 ) ) ;
#20467 = DIRECTION ( 'NONE',  ( 0.000000000000000000, 0.000000000000000000, -1.000000000000000000 ) ) ;
#20468 = DIRECTION ( 'NONE',  ( 0.000000000000000000, 0.000000000000000000, 1.000000000000000000 ) ) ;
#20469 = CARTESIAN_POINT ( 'NONE',  ( -2.999999999999995559, 0.000000000000000000, 0.000000000000000000 ) ) ;
#20470 = LINE ( 'NONE', #3799, #5540 ) ;
#20471 = CARTESIAN_POINT ( 'NONE',  ( 145.0000000000000284, -500.0000000000000000, -29.99999999999997158 ) ) ;
#20472 = EDGE_CURVE ( 'NONE', #6476, #3010, #23672, .T. ) ;
#20473 = CARTESIAN_POINT ( 'NONE',  ( -4.000000000000000000, -1.560351142792950618, -0.2242961665059814425 ) ) ;
#20474 = FACE_OUTER_BOUND ( 'NONE', #4500, .T. ) ;
#20475 = APPLICATION_CONTEXT ( 'automotive_design' ) ;
#20476 = ORIENTED_EDGE ( 'NONE', *, *, #7429, .F. ) ;
#20477 =( NAMED_UNIT ( * ) SI_UNIT ( $, .STERADIAN. ) SOLID_ANGLE_UNIT ( ) );
#20478 = FACE_OUTER_BOUND ( 'NONE', #21795, .T. ) ;
#20479 = CARTESIAN_POINT ( 'NONE',  ( -2.100000000000000089, 2.571758278209441957E-16, -4.694516984716113228 ) ) ;
#20480 = VERTEX_POINT ( 'NONE', #16219 ) ;
#20481 = DIRECTION ( 'NONE',  ( -0.000000000000000000, 0.000000000000000000, -1.000000000000000000 ) ) ;
#20482 = LINE ( 'NONE', #5763, #14244 ) ;
#20483 = CARTESIAN_POINT ( 'NONE',  ( 282.0873946496628264, 268.5095819834011195, -146.1815513148989112 ) ) ;
#20484 = ORIENTED_EDGE ( 'NONE', *, *, #13202, .T. ) ;
#20485 = CARTESIAN_POINT ( 'NONE',  ( 1.500000000000001332, 0.000000000000000000, 6.500000000000000888 ) ) ;
#20486 = CARTESIAN_POINT ( 'NONE',  ( 3.280815508853482498, 7.221948645665444921, -7.591546097228400569 ) ) ;
#20487 = LINE ( 'NONE', #15091, #16558 ) ;
#20488 = VERTEX_POINT ( 'NONE', #9078 ) ;
#20489 = EDGE_CURVE ( 'NONE', #6750, #18313, #14996, .T. ) ;
#20490 = CARTESIAN_POINT ( 'NONE',  ( 2.500000000000000000, 1.178949249685213863, -2.042000000000001148 ) ) ;
#20491 = LINE ( 'NONE', #5884, #19996 ) ;
#20492 = ADVANCED_FACE ( 'NONE', ( #6904 ), #1806, .T. ) ;
#20493 = DIRECTION ( 'NONE',  ( 0.000000000000000000, 0.000000000000000000, 1.000000000000000000 ) ) ;
#20494 = ORIENTED_EDGE ( 'NONE', *, *, #4634, .F. ) ;
#20495 = DIRECTION ( 'NONE',  ( 0.000000000000000000, 0.000000000000000000, -1.000000000000000000 ) ) ;
#20496 = SHAPE_DEFINITION_REPRESENTATION ( #23064, #11474 ) ;
#20497 = FACE_OUTER_BOUND ( 'NONE', #8543, .T. ) ;
#20498 = ADVANCED_FACE ( 'NONE', ( #16562 ), #5327, .F. ) ;
#20499 = CARTESIAN_POINT ( 'NONE',  ( -7.169303301815100227, 4.521054846639364300, -7.349897473154783256 ) ) ;
#20500 = CARTESIAN_POINT ( 'NONE',  ( 4.000000000000000000, 2.309401076758497151, -5.000000000000000000 ) ) ;
#20501 = EDGE_CURVE ( 'NONE', #12981, #19833, #8044, .T. ) ;
#20502 = EDGE_LOOP ( 'NONE', ( #22206, #20413 ) ) ;
#20503 = ORIENTED_EDGE ( 'NONE', *, *, #2934, .T. ) ;
#20504 = CARTESIAN_POINT ( 'NONE',  ( 12.52876685377503918, -21.69578997558838651, 145.0000119999999697 ) ) ;
#20505 = DIRECTION ( 'NONE',  ( 6.753181414994864868E-15, 0.000000000000000000, -1.000000000000000000 ) ) ;
#20506 = CARTESIAN_POINT ( 'NONE',  ( 45.00000000000002132, -52.79999999999936477, 140.0000000000001990 ) ) ;
#20507 = CARTESIAN_POINT ( 'NONE',  ( -127.5331898753161681, 88.09262935741045908, 27.57867027829822959 ) ) ;
#20508 = ADVANCED_BREP_SHAPE_REPRESENTATION ( '', ( #12057, #11210 ), #21934 ) ;
#20509 = EDGE_LOOP ( 'NONE', ( #23409, #4576, #2671, #10940 ) ) ;
#20510 = CYLINDRICAL_SURFACE ( 'NONE', #11413, 5.249999999999973355 ) ;
#20511 = VECTOR ( 'NONE', #250, 1000.000000000000000 ) ;
#20512 = EDGE_LOOP ( 'NONE', ( #23676, #16114, #2759, #3274 ) ) ;
#20513 = LINE ( 'NONE', #15118, #8676 ) ;
#20514 = DIRECTION ( 'NONE',  ( -0.000000000000000000, -1.177509268541832635E-16, 1.000000000000000000 ) ) ;
#20515 = ORIENTED_EDGE ( 'NONE', *, *, #15338, .F. ) ;
#20516 = CARTESIAN_POINT ( 'NONE',  ( -129.1300454301534444, 85.73470730629067305, -28.73951976925631868 ) ) ;
#20517 = CARTESIAN_POINT ( 'NONE',  ( 2.000000000000008882, 3.464101615137749945, 0.000000000000000000 ) ) ;
#20518 = ADVANCED_FACE ( 'NONE', ( #9201 ), #12860, .F. ) ;
#20519 = CARTESIAN_POINT ( 'NONE',  ( 24.20041621714723590, -1006.482064212728119, 145.0000119999999697 ) ) ;
#20520 = EDGE_CURVE ( 'NONE', #12822, #13119, #23436, .T. ) ;
#20521 = CARTESIAN_POINT ( 'NONE',  ( 287.4000000000013415, -127.0000000000000568, -146.4928932188134070 ) ) ;
#20522 = CARTESIAN_POINT ( 'NONE',  ( 7.264118654998712898, -4.945491722146229563, -7.907633014911220393 ) ) ;
#20523 = CARTESIAN_POINT ( 'NONE',  ( 93.00000000000000000, 76.26794919243113213, 2.999999999999975131 ) ) ;
#20524 = CARTESIAN_POINT ( 'NONE',  ( -145.0000000000000284, -1.110223024625156540E-13, 90.00000000000000000 ) ) ;
#20525 = ORIENTED_EDGE ( 'NONE', *, *, #17142, .F. ) ;
#20526 = ADVANCED_FACE ( 'NONE', ( #3508 ), #3610, .T. ) ;
#20527 = CARTESIAN_POINT ( 'NONE',  ( -282.2000000000010118, 9.787860418609727755E-13, 0.000000000000000000 ) ) ;
#20528 = DIRECTION ( 'NONE',  ( 0.9289202219288174023, 0.3702799228849934510, 6.982962677686266711E-15 ) ) ;
#20529 = AXIS2_PLACEMENT_3D ( 'NONE', #15951, #15845, #21131 ) ;
#20531 = ORIENTED_EDGE ( 'NONE', *, *, #21929, .F. ) ;
#20530 = ORIENTED_EDGE ( 'NONE', *, *, #23695, .T. ) ;
#20532 = EDGE_CURVE ( 'NONE', #2917, #10831, #19816, .T. ) ;
#20533 = FACE_OUTER_BOUND ( 'NONE', #9317, .T. ) ;
#20534 = DIRECTION ( 'NONE',  ( 0.000000000000000000, -1.000000000000000000, 0.000000000000000000 ) ) ;
#20535 = EDGE_CURVE ( 'NONE', #4200, #15958, #13848, .T. ) ;
#20536 = ORIENTED_EDGE ( 'NONE', *, *, #14512, .F. ) ;
#20537 = CARTESIAN_POINT ( 'NONE',  ( -134.6777706902592229, -1076.726150876685551, 31.11671059283538554 ) ) ;
#20538 = ORIENTED_EDGE ( 'NONE', *, *, #14524, .T. ) ;
#20539 = FACE_OUTER_BOUND ( 'NONE', #5268, .T. ) ;
#20540 = ORIENTED_EDGE ( 'NONE', *, *, #1679, .T. ) ;
#20541 = CARTESIAN_POINT ( 'NONE',  ( -281.4928932188134354, 267.8000000000000114, -150.1999999999999318 ) ) ;
#20542 = CARTESIAN_POINT ( 'NONE',  ( 119.6158142514525622, -1087.367367941136990, -29.99999999999356604 ) ) ;
#20543 = ORIENTED_EDGE ( 'NONE', *, *, #6460, .F. ) ;
#20544 = AXIS2_PLACEMENT_3D ( 'NONE', #4689, #4800, #3107 ) ;
#20545 = EDGE_CURVE ( 'NONE', #14560, #442, #8417, .T. ) ;
#20546 = FACE_OUTER_BOUND ( 'NONE', #54, .T. ) ;
#20547 = ORIENTED_EDGE ( 'NONE', *, *, #11016, .T. ) ;
#20548 = CARTESIAN_POINT ( 'NONE',  ( -129.1311602790088102, 85.73302760282668089, 28.74299381080684412 ) ) ;
#20549 = CARTESIAN_POINT ( 'NONE',  ( 0.000000000000000000, 0.000000000000000000, 0.000000000000000000 ) ) ;
#20550 = CARTESIAN_POINT ( 'NONE',  ( -130.4031948627974486, 44.80746418436699940, -90.00000000000000000 ) ) ;
#20551 = DIRECTION ( 'NONE',  ( 1.000000000000000000, 0.000000000000000000, 0.000000000000000000 ) ) ;
#20552 = ORIENTED_EDGE ( 'NONE', *, *, #13451, .T. ) ;
#20553 = CARTESIAN_POINT ( 'NONE',  ( -280.6220388411722411, 269.5592670532760167, -146.3520027839447835 ) ) ;
#20554 = CARTESIAN_POINT ( 'NONE',  ( 2.700000000000001510, 0.000000000000000000, 0.000000000000000000 ) ) ;
#20555 = VECTOR ( 'NONE', #4218, 1000.000000000000000 ) ;
#20556 = ORIENTED_EDGE ( 'NONE', *, *, #7978, .F. ) ;
#20557 = VECTOR ( 'NONE', #16350, 1000.000000000000000 ) ;
#20558 = CARTESIAN_POINT ( 'NONE',  ( -2.775557561562891351E-14, 290.0000000000000000, 0.000000000000000000 ) ) ;
#20559 = ADVANCED_FACE ( 'NONE', ( #19932 ), #3383, .F. ) ;
#20560 = DIRECTION ( 'NONE',  ( -1.000000000000000000, 0.000000000000000000, -0.000000000000000000 ) ) ;
#20561 = CARTESIAN_POINT ( 'NONE',  ( 132.0350058597971952, 81.18997658688611807, -27.99555145635497411 ) ) ;
#20562 = EDGE_CURVE ( 'NONE', #21142, #3965, #19315, .T. ) ;
#20563 = EDGE_CURVE ( 'NONE', #5669, #12251, #11386, .T. ) ;
#20564 = CARTESIAN_POINT ( 'NONE',  ( 284.5436892194421148, 270.4188186979286002, 145.9952621458756710 ) ) ;
#20565 = CARTESIAN_POINT ( 'NONE',  ( -285.0938770989753834, 269.1689414351989740, -146.2440776823445390 ) ) ;
#20566 = CARTESIAN_POINT ( 'NONE',  ( -129.2206655591605511, -1072.408698320350595, 30.00000000000641620 ) ) ;
#20567 = CARTESIAN_POINT ( 'NONE',  ( 123.5476367174099011, -1093.600214943837045, 31.99235058689527733 ) ) ;
#20568 = ORIENTED_EDGE ( 'NONE', *, *, #10036, .T. ) ;
#20570 = DIRECTION ( 'NONE',  ( 0.000000000000000000, 0.000000000000000000, 1.000000000000000000 ) ) ;
#20569 = AXIS2_PLACEMENT_3D ( 'NONE', #10528, #1667, #3354 ) ;
#20571 = VERTEX_POINT ( 'NONE', #22210 ) ;
#20572 = DIRECTION ( 'NONE',  ( -1.000000000000000000, 0.000000000000000000, 0.000000000000000000 ) ) ;
#20573 = VECTOR ( 'NONE', #13272, 1000.000000000000000 ) ;
#20574 = FACE_OUTER_BOUND ( 'NONE', #20343, .T. ) ;
#20575 = DIRECTION ( 'NONE',  ( 0.000000000000000000, 0.000000000000000000, 1.000000000000000000 ) ) ;
#20576 = ORIENTED_EDGE ( 'NONE', *, *, #8678, .F. ) ;
#20577 = CYLINDRICAL_SURFACE ( 'NONE', #16549, 2.649999999999971934 ) ;
#20578 = DIRECTION ( 'NONE',  ( 0.000000000000000000, 0.000000000000000000, 1.000000000000000000 ) ) ;
#20579 = DIRECTION ( 'NONE',  ( -3.495664435217746592E-15, -1.000000000000000000, 0.000000000000000000 ) ) ;
#20580 = CARTESIAN_POINT ( 'NONE',  ( -129.2206655591611764, -1072.408698320350140, -32.05499999999358351 ) ) ;
#20581 = DIRECTION ( 'NONE',  ( 1.350636282998972974E-14, 0.000000000000000000, -1.000000000000000000 ) ) ;
#20582 = CARTESIAN_POINT ( 'NONE',  ( -64.99999999999998579, -52.79999999999942872, 125.0000000000001421 ) ) ;
#20583 = CARTESIAN_POINT ( 'NONE',  ( -72.64999999999996305, -112.6666666666667140, 144.9999999999999716 ) ) ;
#20584 = ORIENTED_EDGE ( 'NONE', *, *, #2033, .F. ) ;
#20585 =( LENGTH_UNIT ( ) NAMED_UNIT ( * ) SI_UNIT ( .MILLI., .METRE. ) );
#20586 = DIRECTION ( 'NONE',  ( -0.000000000000000000, 1.000000000000000000, -3.469446951953613794E-15 ) ) ;
#20587 = DIRECTION ( 'NONE',  ( 1.000000000000000000, 0.000000000000000000, 0.000000000000000000 ) ) ;
#20588 = ORIENTED_EDGE ( 'NONE', *, *, #179, .T. ) ;
#20589 = ORIENTED_EDGE ( 'NONE', *, *, #6365, .F. ) ;
#20590 = VECTOR ( 'NONE', #3201, 1000.000000000000000 ) ;
#20591 = DIRECTION ( 'NONE',  ( 1.000000000000000000, 0.000000000000000000, 0.000000000000000000 ) ) ;
#20593 = VECTOR ( 'NONE', #9112, 1000.000000000000000 ) ;
#20592 = DIRECTION ( 'NONE',  ( 0.000000000000000000, 0.000000000000000000, 1.000000000000000000 ) ) ;
#20594 = CIRCLE ( 'NONE', #4010, 5.249999999999949374 ) ;
#20595 = CARTESIAN_POINT ( 'NONE',  ( 0.000000000000000000, 0.000000000000000000, 169.9999999999999716 ) ) ;
#20596 = EDGE_LOOP ( 'NONE', ( #4556, #18569, #12467, #6950 ) ) ;
#20597 = DIRECTION ( 'NONE',  ( 1.000000000000000000, 0.000000000000000000, 0.000000000000000000 ) ) ;
#20598 = FACE_BOUND ( 'NONE', #22447, .T. ) ;
#20599 = CARTESIAN_POINT ( 'NONE',  ( 34.99999999999999289, 2.789133085058097101E-16, -2.055000000000000160 ) ) ;
#20600 = VERTEX_POINT ( 'NONE', #6036 ) ;
#20601 = CARTESIAN_POINT ( 'NONE',  ( 4.207491450040567571, -2.029819825146485179, -3.671670828759567407 ) ) ;
#20602 = CARTESIAN_POINT ( 'NONE',  ( 100.0000000000000000, 269.9999999999999432, 145.0000000000000284 ) ) ;
#20603 = CARTESIAN_POINT ( 'NONE',  ( 2.500000000000000000, 1.178949249685213863, -2.042000000000001148 ) ) ;
#20604 = ORIENTED_EDGE ( 'NONE', *, *, #21867, .T. ) ;
#20605 = DIRECTION ( 'NONE',  ( 0.000000000000000000, 0.000000000000000000, -1.000000000000000000 ) ) ;
#20606 = APPLICATION_PROTOCOL_DEFINITION ( 'draft international standard', 'automotive_design', 1998, #22932 ) ;
#20607 = DIRECTION ( 'NONE',  ( 1.000000000000000000, -3.051161311199799893E-31, -8.144298233840332611E-17 ) ) ;
#20608 = CIRCLE ( 'NONE', #7070, 2.649999999999985700 ) ;
#20609 = DIRECTION ( 'NONE',  ( -0.000000000000000000, 1.000000000000000000, -3.469446951953613794E-15 ) ) ;
#20610 = CARTESIAN_POINT ( 'NONE',  ( -100.0000000000000000, 269.9999999999999432, 145.0000000000000284 ) ) ;
#20611 = AXIS2_PLACEMENT_3D ( 'NONE', #6419, #19437, #13824 ) ;
#20612 = VERTEX_POINT ( 'NONE', #249 ) ;
#20613 = ORIENTED_EDGE ( 'NONE', *, *, #3733, .F. ) ;
#20614 = CARTESIAN_POINT ( 'NONE',  ( -3.000000000000002665, 3.043247295881173007E-15, 24.69999999999999929 ) ) ;
#20615 = CYLINDRICAL_SURFACE ( 'NONE', #8703, 145.0000000000000284 ) ;
#20616 = EDGE_CURVE ( 'NONE', #2346, #5614, #7855, .T. ) ;
#20617 = AXIS2_PLACEMENT_3D ( 'NONE', #480, #15220, #7587 ) ;
#20618 = UNCERTAINTY_MEASURE_WITH_UNIT (LENGTH_MEASURE( 1.000000000000000082E-05 ), #23236, 'distance_accuracy_value', 'NONE');
#20619 = EDGE_CURVE ( 'NONE', #13591, #14699, #8094, .T. ) ;
#20620 = EDGE_CURVE ( 'NONE', #766, #11911, #3735, .T. ) ;
#20621 = ORIENTED_EDGE ( 'NONE', *, *, #734, .F. ) ;
#20622 = CARTESIAN_POINT ( 'NONE',  ( -4.403473400622099909, -6.117907484625868975, -5.839445138371144960E-15 ) ) ;
#20623 = AXIS2_PLACEMENT_3D ( 'NONE', #11999, #19304, #2764 ) ;
#20624 = FACE_OUTER_BOUND ( 'NONE', #1817, .T. ) ;
#20625 = ORIENTED_EDGE ( 'NONE', *, *, #10516, .T. ) ;
#20626 = DIRECTION ( 'NONE',  ( 0.000000000000000000, 0.000000000000000000, 1.000000000000000000 ) ) ;
#20627 = EDGE_CURVE ( 'NONE', #14650, #16878, #11278, .T. ) ;
#20628 = CIRCLE ( 'NONE', #18689, 145.0000000000000284 ) ;
#20629 = CLOSED_SHELL ( 'NONE', ( #22232, #7529, #9931, #6663, #8280, #3506, #19288, #4286, #6049, #12041, #7729, #4851, #18737, #11494, #6570, #4554, #15588, #14809, #13382, #5054, #18616, #616, #20353, #21798, #11182, #18451, #16009 ) ) ;
#20630 = ORIENTED_EDGE ( 'NONE', *, *, #15047, .F. ) ;
#20631 = DIRECTION ( 'NONE',  ( 1.000000000000000000, 0.000000000000000000, 0.000000000000000000 ) ) ;
#20632 = FACE_OUTER_BOUND ( 'NONE', #20852, .T. ) ;
#20633 = VERTEX_POINT ( 'NONE', #16791 ) ;
#20634 = ORIENTED_EDGE ( 'NONE', *, *, #6574, .T. ) ;
#20635 = DIRECTION ( 'NONE',  ( -0.000000000000000000, 0.000000000000000000, 1.000000000000000000 ) ) ;
#20636 = CARTESIAN_POINT ( 'NONE',  ( -280.6222583006965010, 271.9268706878667103, -148.1682701916305973 ) ) ;
#20637 = VECTOR ( 'NONE', #14815, 1000.000000000000000 ) ;
#20638 = DIRECTION ( 'NONE',  ( 1.000000000000000000, 0.000000000000000000, 0.000000000000000000 ) ) ;
#20639 = FACE_OUTER_BOUND ( 'NONE', #20074, .T. ) ;
#20640 = CARTESIAN_POINT ( 'NONE',  ( 23.72315261474500048, -991.9446085409455236, 145.0000119999999697 ) ) ;
#20641 = CARTESIAN_POINT ( 'NONE',  ( 2.500000000000002220, -1.178949249685215417, 2.042000000000002036 ) ) ;
#20642 = AXIS2_PLACEMENT_3D ( 'NONE', #967, #15724, #6655 ) ;
#20643 = DIRECTION ( 'NONE',  ( -1.000000000000000000, -0.000000000000000000, -0.000000000000000000 ) ) ;
#20644 = ORIENTED_EDGE ( 'NONE', *, *, #15117, .F. ) ;
#20645 = FACE_BOUND ( 'NONE', #18374, .T. ) ;
#20646 = CARTESIAN_POINT ( 'NONE',  ( -288.2000000000008981, 35.00000000000100897, 105.0000000000000000 ) ) ;
#20647 =( LENGTH_UNIT ( ) NAMED_UNIT ( * ) SI_UNIT ( .MILLI., .METRE. ) );
#20648 = VECTOR ( 'NONE', #8990, 1000.000000000000000 ) ;
#20650 = ORIENTED_EDGE ( 'NONE', *, *, #1946, .T. ) ;
#20649 = ORIENTED_EDGE ( 'NONE', *, *, #18932, .T. ) ;
#20651 = DIRECTION ( 'NONE',  ( 1.000000000000000000, 0.000000000000000000, 0.000000000000000000 ) ) ;
#20652 = DIRECTION ( 'NONE',  ( 0.000000000000000000, 0.000000000000000000, 1.000000000000000000 ) ) ;
#20653 = ORIENTED_EDGE ( 'NONE', *, *, #3116, .T. ) ;
#20654 = ADVANCED_FACE ( 'NONE', ( #14999 ), #22342, .T. ) ;
#20655 = DIRECTION ( 'NONE',  ( -1.000000000000000000, 1.408839003528726857E-14, 6.982962677686266711E-15 ) ) ;
#20656 = VERTEX_POINT ( 'NONE', #2162 ) ;
#20657 = CIRCLE ( 'NONE', #14913, 2.649999999999985700 ) ;
#20658 = EDGE_CURVE ( 'NONE', #22534, #20268, #19580, .T. ) ;
#20659 = CYLINDRICAL_SURFACE ( 'NONE', #12304, 23.97500000000000497 ) ;
#20660 = ADVANCED_FACE ( 'NONE', ( #20639 ), #13090, .T. ) ;
#20661 = ORIENTED_EDGE ( 'NONE', *, *, #2615, .F. ) ;
#20662 = DIRECTION ( 'NONE',  ( 0.000000000000000000, 1.000000000000000000, 1.177509268541832635E-16 ) ) ;
#20663 = ORIENTED_EDGE ( 'NONE', *, *, #4109, .F. ) ;
#20664 = EDGE_CURVE ( 'NONE', #2537, #8393, #9985, .T. ) ;
#20665 = PRODUCT_DEFINITION ( 'UNKNOWN', '', #11615, #7589 ) ;
#20666 = PLANE ( 'NONE',  #14146 ) ;
#20667 = ORIENTED_EDGE ( 'NONE', *, *, #15972, .T. ) ;
#20668 = EDGE_CURVE ( 'NONE', #21528, #1506, #19642, .T. ) ;
#20669 = CARTESIAN_POINT ( 'NONE',  ( -22.46865867768271841, -988.9158635398115393, -145.0000000000001137 ) ) ;
#20670 = CARTESIAN_POINT ( 'NONE',  ( -0.6937372685066653943, 4.453844082567723461, -3.610536846335889116 ) ) ;
#20671 = DIRECTION ( 'NONE',  ( 0.000000000000000000, 0.000000000000000000, -1.000000000000000000 ) ) ;
#20672 = DIRECTION ( 'NONE',  ( -1.000000000000000000, 0.000000000000000000, 0.000000000000000000 ) ) ;
#20673 = VERTEX_POINT ( 'NONE', #17958 ) ;
#20674 = CARTESIAN_POINT ( 'NONE',  ( -280.9952621458755857, 268.8927021017107108, -146.8958543268122128 ) ) ;
#20675 = VECTOR ( 'NONE', #1358, 1000.000000000000000 ) ;
#20676 = ORIENTED_EDGE ( 'NONE', *, *, #8723, .T. ) ;
#20677 = DIRECTION ( 'NONE',  ( -6.982962677686266711E-15, 9.837870180509810443E-29, -1.000000000000000000 ) ) ;
#20678 = AXIS2_PLACEMENT_3D ( 'NONE', #4019, #22498, #5967 ) ;
#20679 = CARTESIAN_POINT ( 'NONE',  ( 0.000000000000000000, 0.000000000000000000, -90.00000000000000000 ) ) ;
#20680 = DIRECTION ( 'NONE',  ( -0.000000000000000000, -0.000000000000000000, -1.000000000000000000 ) ) ;
#20681 = CARTESIAN_POINT ( 'NONE',  ( 282.1427398886702917, 268.3758453455903918, 146.2440776823445958 ) ) ;
#20682 = DIRECTION ( 'NONE',  ( 0.000000000000000000, -2.618450529776313049E-15, -1.000000000000000000 ) ) ;
#20683 = ORIENTED_EDGE ( 'NONE', *, *, #5095, .F. ) ;
#20684 = VECTOR ( 'NONE', #1213, 1000.000000000000000 ) ;
#20685 = DIRECTION ( 'NONE',  ( 0.000000000000000000, 0.4999999999999979461, -0.8660254037844397068 ) ) ;
#20686 = VECTOR ( 'NONE', #3143, 1000.000000000000000 ) ;
#20687 = CARTESIAN_POINT ( 'NONE',  ( 155.0000000000000284, -209.9999999999996874, 27.50000000000647660 ) ) ;
#20688 = DIRECTION ( 'NONE',  ( 0.000000000000000000, 1.000000000000000000, 1.177509268541832635E-16 ) ) ;
#20689 = CONTEXT_DEPENDENT_SHAPE_REPRESENTATION ( #22804, #12235 ) ;
#20690 = EDGE_LOOP ( 'NONE', ( #19786, #8083, #6391, #12975 ) ) ;
#20691 = FACE_OUTER_BOUND ( 'NONE', #1428, .T. ) ;
#20692 = EDGE_LOOP ( 'NONE', ( #12642, #12768 ) ) ;
#20693 = FACE_OUTER_BOUND ( 'NONE', #18163, .T. ) ;
#20694 = CARTESIAN_POINT ( 'NONE',  ( -20.00000000000000000, 2.449293598294706513E-15, -150.0000000000000000 ) ) ;
#20695 = EDGE_CURVE ( 'NONE', #10625, #20887, #23153, .T. ) ;
#20696 = ADVANCED_FACE ( 'NONE', ( #15923 ), #2533, .T. ) ;
#20697 = ORIENTED_EDGE ( 'NONE', *, *, #13037, .T. ) ;
#20698 = EDGE_CURVE ( 'NONE', #14308, #17543, #1474, .T. ) ;
#20699 = DIRECTION ( 'NONE',  ( 1.110223024625157172E-14, 0.000000000000000000, -1.000000000000000000 ) ) ;
#20700 = ORIENTED_EDGE ( 'NONE', *, *, #12996, .F. ) ;
#20701 = DIRECTION ( 'NONE',  ( -1.000000000000000000, -0.000000000000000000, -0.000000000000000000 ) ) ;
#20702 = CYLINDRICAL_SURFACE ( 'NONE', #4143, 5.249999999999973355 ) ;
#20703 = DIRECTION ( 'NONE',  ( 0.000000000000000000, 0.000000000000000000, -1.000000000000000000 ) ) ;
#20704 = FACE_OUTER_BOUND ( 'NONE', #14373, .T. ) ;
#20705 = DIRECTION ( 'NONE',  ( -1.000000000000000000, 0.000000000000000000, 0.000000000000000000 ) ) ;
#20706 = CARTESIAN_POINT ( 'NONE',  ( -59.99999999999995737, -59.79999999999975557, 74.99940828143398619 ) ) ;
#20707 = VECTOR ( 'NONE', #4073, 1000.000000000000114 ) ;
#20708 = CARTESIAN_POINT ( 'NONE',  ( 0.2500000000000002220, 0.000000000000000000, 4.000000000000000000 ) ) ;
#20709 = VERTEX_POINT ( 'NONE', #18079 ) ;
#20710 = LINE ( 'NONE', #7923, #14573 ) ;
#20711 = AXIS2_PLACEMENT_3D ( 'NONE', #9537, #13207, #22321 ) ;
#20712 = CARTESIAN_POINT ( 'NONE',  ( -122.8605704798723224, 82.74225173005862644, 27.94500000000641649 ) ) ;
#20713 = VECTOR ( 'NONE', #21993, 1000.000000000000000 ) ;
#20714 = ORIENTED_EDGE ( 'NONE', *, *, #22555, .T. ) ;
#20715 = EDGE_LOOP ( 'NONE', ( #17953, #17331, #21763, #20630, #14872 ) ) ;
#20716 = CARTESIAN_POINT ( 'NONE',  ( -37.61698748598617215, 140.0355749532209586, -90.00000000000000000 ) ) ;
#20717 = CARTESIAN_POINT ( 'NONE',  ( -93.00000000000000000, -152.9999999999996874, 129.9038105676659711 ) ) ;
#20718 = DIRECTION ( 'NONE',  ( -1.000000000000000000, -0.000000000000000000, -0.000000000000000000 ) ) ;
#20719 = ORIENTED_EDGE ( 'NONE', *, *, #7716, .F. ) ;
#20720 = DIRECTION ( 'NONE',  ( -1.000000000000000000, 0.000000000000000000, 0.000000000000000000 ) ) ;
#20721 = LINE ( 'NONE', #811, #10532 ) ;
#20722 = AXIS2_PLACEMENT_3D ( 'NONE', #23362, #17461, #905 ) ;
#20723 = DIRECTION ( 'NONE',  ( 1.000000000000000000, 0.000000000000000000, 0.000000000000000000 ) ) ;
#20724 = ORIENTED_EDGE ( 'NONE', *, *, #9111, .T. ) ;
#20725 = DIRECTION ( 'NONE',  ( 0.000000000000000000, 0.000000000000000000, 1.000000000000000000 ) ) ;
#20726 = CYLINDRICAL_SURFACE ( 'NONE', #3409, 2.649999999999971934 ) ;
#20727 = CONICAL_SURFACE ( 'NONE', #10346, 2.055000000000001492, 0.7853981633974633780 ) ;
#20728 = UNCERTAINTY_MEASURE_WITH_UNIT (LENGTH_MEASURE( 1.000000000000000082E-05 ), #18486, 'distance_accuracy_value', 'NONE');
#20729 = SURFACE_STYLE_USAGE ( .BOTH. , #581 ) ;
#20730 = VECTOR ( 'NONE', #15180, 1000.000000000000000 ) ;
#20731 = VERTEX_POINT ( 'NONE', #4920 ) ;
#20732 = CARTESIAN_POINT ( 'NONE',  ( -64.99999999999995737, -52.79999999999965610, 65.00000000000017053 ) ) ;
#20733 = AXIS2_PLACEMENT_3D ( 'NONE', #3279, #10689, #16337 ) ;
#20734 = FACE_BOUND ( 'NONE', #12557, .T. ) ;
#20735 = CARTESIAN_POINT ( 'NONE',  ( -31.74999999999995737, 0.000000000000000000, 5.000000000000001776 ) ) ;
#20736 = DIRECTION ( 'NONE',  ( -1.110223024625155594E-14, 0.000000000000000000, -1.000000000000000000 ) ) ;
#20737 = ORIENTED_EDGE ( 'NONE', *, *, #23587, .T. ) ;
#20738 = ORIENTED_EDGE ( 'NONE', *, *, #20348, .T. ) ;
#20739 = DIRECTION ( 'NONE',  ( 0.000000000000000000, 0.000000000000000000, -1.000000000000000000 ) ) ;
#20740 = DIRECTION ( 'NONE',  ( 0.000000000000000000, 0.000000000000000000, -1.000000000000000000 ) ) ;
#20741 = VECTOR ( 'NONE', #11548, 1000.000000000000114 ) ;
#20742 = VECTOR ( 'NONE', #7024, 1000.000000000000000 ) ;
#20743 = AXIS2_PLACEMENT_3D ( 'NONE', #15088, #17008, #22530 ) ;
#20744 = VECTOR ( 'NONE', #16657, 1000.000000000000000 ) ;
#20745 = ORIENTED_EDGE ( 'NONE', *, *, #13037, .F. ) ;
#20746 = LINE ( 'NONE', #9536, #7480 ) ;
#20747 = DIRECTION ( 'NONE',  ( 0.000000000000000000, 0.000000000000000000, 1.000000000000000000 ) ) ;
#20748 = ORIENTED_EDGE ( 'NONE', *, *, #13754, .T. ) ;
#20749 = FACE_OUTER_BOUND ( 'NONE', #21290, .T. ) ;
#20750 = ADVANCED_FACE ( 'NONE', ( #6170 ), #1179, .F. ) ;
#20751 = ORIENTED_EDGE ( 'NONE', *, *, #6202, .T. ) ;
#20752 = DIRECTION ( 'NONE',  ( 3.495664435217746987E-15, -1.000000000000000000, -0.000000000000000000 ) ) ;
#20753 = DIRECTION ( 'NONE',  ( 0.000000000000000000, -0.000000000000000000, 1.000000000000000000 ) ) ;
#20754 = ORIENTED_EDGE ( 'NONE', *, *, #9762, .T. ) ;
#20755 = ORIENTED_EDGE ( 'NONE', *, *, #4332, .F. ) ;
#20756 = CARTESIAN_POINT ( 'NONE',  ( 0.5636800770130377947, 4.293361309317166530, -3.531542292954102713 ) ) ;
#20757 = EDGE_CURVE ( 'NONE', #12610, #11181, #17279, .T. ) ;
#20758 = MECHANICAL_DESIGN_GEOMETRIC_PRESENTATION_REPRESENTATION (  '', ( #10770 ), #14627 ) ;
#20759 = CYLINDRICAL_SURFACE ( 'NONE', #3470, 2.649999999999985700 ) ;
#20760 = AXIS2_PLACEMENT_3D ( 'NONE', #18642, #4165, #9501 ) ;
#20761 = CARTESIAN_POINT ( 'NONE',  ( 281.4928932188133786, 267.8000000000000114, -147.1999999999999318 ) ) ;
#20762 = ADVANCED_FACE ( 'NONE', ( #17841 ), #14127, .T. ) ;
#20763 = AXIS2_PLACEMENT_3D ( 'NONE', #10738, #3330, #21699 ) ;
#20764 = CARTESIAN_POINT ( 'NONE',  ( 284.9329465209281693, 269.4795879751484904, 146.1810844504668125 ) ) ;
#20765 = DIRECTION ( 'NONE',  ( 0.000000000000000000, 0.000000000000000000, -1.000000000000000000 ) ) ;
#20766 = CARTESIAN_POINT ( 'NONE',  ( 2.500000000000002220, 2.357898499370434386, -3.469446951953614189E-15 ) ) ;
#20767 = VECTOR ( 'NONE', #14414, 1000.000000000000000 ) ;
#20768 = LINE ( 'NONE', #2536, #13140 ) ;
#20769 = VERTEX_POINT ( 'NONE', #1288 ) ;
#20770 = DIRECTION ( 'NONE',  ( -3.495664435217746987E-15, -1.000000000000000000, 0.000000000000000000 ) ) ;
#20771 = FACE_OUTER_BOUND ( 'NONE', #23555, .T. ) ;
#20772 = EDGE_CURVE ( 'NONE', #17208, #640, #6619, .T. ) ;
#20773 = TOROIDAL_SURFACE ( 'NONE', #9601, 4.000000000000000000, 0.2500000000000000000 ) ;
#20774 = VERTEX_POINT ( 'NONE', #12333 ) ;
#20775 = CARTESIAN_POINT ( 'NONE',  ( -136.3934655611484743, -1073.633154336008602, -32.17346063704741965 ) ) ;
#20776 = CARTESIAN_POINT ( 'NONE',  ( 280.6220388411722411, 269.5592670532759598, -146.3520027839447550 ) ) ;
#20777 = ORIENTED_EDGE ( 'NONE', *, *, #13496, .T. ) ;
#20778 = AXIS2_PLACEMENT_3D ( 'NONE', #10704, #20304, #13003 ) ;
#20779 = CARTESIAN_POINT ( 'NONE',  ( -35.00000000000001421, 90.00000000000001421, 0.000000000000000000 ) ) ;
#20781 = AXIS2_PLACEMENT_3D ( 'NONE', #14527, #18144, #14649 ) ;
#20780 = COLOUR_RGB ( '',1.000000000000000000, 0.9490196078431372140, 0.9098039215686274384 ) ;
#20782 = VERTEX_POINT ( 'NONE', #19068 ) ;
#20783 = AXIS2_PLACEMENT_3D ( 'NONE', #17575, #909, #1389 ) ;
#20784 = VECTOR ( 'NONE', #1343, 1000.000000000000000 ) ;
#20785 = DIRECTION ( 'NONE',  ( -1.000000000000000000, 0.000000000000000000, 0.000000000000000000 ) ) ;
#20786 = CIRCLE ( 'NONE', #10790, 2.649999999999985700 ) ;
#20787 = CARTESIAN_POINT ( 'NONE',  ( 283.0299054689546665, 272.0295083325147516, -145.5908103165959631 ) ) ;
#20788 = COLOUR_RGB ( '',1.000000000000000000, 0.9490196078431372140, 0.9098039215686274384 ) ;
#20789 = AXIS2_PLACEMENT_3D ( 'NONE', #14842, #22421, #4055 ) ;
#20790 = ORIENTED_EDGE ( 'NONE', *, *, #16670, .T. ) ;
#20791 = DIRECTION ( 'NONE',  ( -0.000000000000000000, -0.000000000000000000, 1.000000000000000000 ) ) ;
#20792 =( LENGTH_UNIT ( ) NAMED_UNIT ( * ) SI_UNIT ( .MILLI., .METRE. ) );
#20793 = ORIENTED_EDGE ( 'NONE', *, *, #5584, .T. ) ;
#20794 =( REPRESENTATION_RELATIONSHIP ('NONE','NONE', #10127, #18083 ) REPRESENTATION_RELATIONSHIP_WITH_TRANSFORMATION ( #11322 )SHAPE_REPRESENTATION_RELATIONSHIP( ) );
#20795 = ADVANCED_FACE ( 'NONE', ( #5156 ), #16038, .F. ) ;
#20796 = DIRECTION ( 'NONE',  ( 1.000000000000000000, 3.736327486719275871E-16, -1.296299001029869881E-30 ) ) ;
#20797 = VERTEX_POINT ( 'NONE', #2967 ) ;
#20798 = CARTESIAN_POINT ( 'NONE',  ( -44.99999999999997868, -52.79999999999937899, 142.6500000000001478 ) ) ;
#20799 = CARTESIAN_POINT ( 'NONE',  ( 89.00000000000000000, -74.99999999999998579, 0.000000000000000000 ) ) ;
#20800 = CARTESIAN_POINT ( 'NONE',  ( 0.000000000000000000, -1000.000000000000000, 90.00000000000000000 ) ) ;
#20801 = PLANE ( 'NONE',  #8069 ) ;
#20802 = ORIENTED_EDGE ( 'NONE', *, *, #9354, .T. ) ;
#20803 = AXIS2_PLACEMENT_3D ( 'NONE', #12269, #17654, #6563 ) ;
#20804 = CARTESIAN_POINT ( 'NONE',  ( -280.0000000000000000, 269.9697000000000457, -144.9999999999999716 ) ) ;
#20805 = SURFACE_STYLE_USAGE ( .BOTH. , #2195 ) ;
#20806 = EDGE_CURVE ( 'NONE', #22426, #22539, #11169, .T. ) ;
#20807 = AXIS2_PLACEMENT_3D ( 'NONE', #22874, #9867, #6343 ) ;
#20808 = VECTOR ( 'NONE', #19862, 1000.000000000000114 ) ;
#20809 = VECTOR ( 'NONE', #974, 1000.000000000000000 ) ;
#20810 = AXIS2_PLACEMENT_3D ( 'NONE', #21796, #10360, #8778 ) ;
#20811 = EDGE_CURVE ( 'NONE', #5315, #21765, #12460, .T. ) ;
#20813 = ORIENTED_EDGE ( 'NONE', *, *, #5661, .T. ) ;
#20812 = ORIENTED_EDGE ( 'NONE', *, *, #1346, .T. ) ;
#20814 = DIRECTION ( 'NONE',  ( 0.000000000000000000, 0.000000000000000000, 1.000000000000000000 ) ) ;
#20815 = CARTESIAN_POINT ( 'NONE',  ( 40.00000000000000000, 100.0000000000000000, 125.0000000000000000 ) ) ;
#20816 = CARTESIAN_POINT ( 'NONE',  ( 131.5858269427386915, 81.91565353609531996, -29.18615827854495848 ) ) ;
#20817 = ADVANCED_FACE ( 'NONE', ( #5055 ), #13585, .F. ) ;
#20818 = FACE_OUTER_BOUND ( 'NONE', #5041, .T. ) ;
#20819 = FACE_BOUND ( 'NONE', #21563, .T. ) ;
#20820 = EDGE_LOOP ( 'NONE', ( #10893, #17638 ) ) ;
#20821 = EDGE_CURVE ( 'NONE', #10033, #8499, #17720, .T. ) ;
#20822 = CYLINDRICAL_SURFACE ( 'NONE', #23421, 2.649999999999999467 ) ;
#20823 = PRODUCT_DEFINITION_FORMATION_WITH_SPECIFIED_SOURCE ( 'ANY', '', #10988, .NOT_KNOWN. ) ;
#20824 = CARTESIAN_POINT ( 'NONE',  ( 0.000000000000000000, -1000.000000000000000, -125.0000000000001137 ) ) ;
#20825 = CARTESIAN_POINT ( 'NONE',  ( 123.2641556675340127, -1093.973169342142455, 28.46749050845384943 ) ) ;
#20826 = AXIS2_PLACEMENT_3D ( 'NONE', #14779, #22475, #5941 ) ;
#20827 = AXIS2_PLACEMENT_3D ( 'NONE', #20173, #18023, #5339 ) ;
#20828 = EDGE_LOOP ( 'NONE', ( #20901, #14968, #15708, #7352 ) ) ;
#20829 = AXIS2_PLACEMENT_3D ( 'NONE', #13558, #17251, #696 ) ;
#20830 = AXIS2_PLACEMENT_3D ( 'NONE', #18520, #20312, #3904 ) ;
#20831 = CARTESIAN_POINT ( 'NONE',  ( 40.00000000000000000, 100.0000000000000000, -150.2000000000005571 ) ) ;
#20832 = ORIENTED_EDGE ( 'NONE', *, *, #9436, .F. ) ;
#20833 = LINE ( 'NONE', #7663, #11838 ) ;
#20834 = CARTESIAN_POINT ( 'NONE',  ( -285.2000000000008981, 35.00000000000100897, 102.3500000000000227 ) ) ;
#20835 = ORIENTED_EDGE ( 'NONE', *, *, #11106, .F. ) ;
#20836 = CARTESIAN_POINT ( 'NONE',  ( 3.750000000000005329, 6.495190528383288253, 0.000000000000000000 ) ) ;
#20837 = EDGE_LOOP ( 'NONE', ( #19777, #22882, #17033, #23400, #15741 ) ) ;
#20838 = CARTESIAN_POINT ( 'NONE',  ( 50.00000000000000000, -59.79999999999974847, 74.99940828143402882 ) ) ;
#20839 = DIRECTION ( 'NONE',  ( -1.000000000000000000, -0.000000000000000000, -0.000000000000000000 ) ) ;
#20840 = CARTESIAN_POINT ( 'NONE',  ( 0.000000000000000000, 1.865214261513747767E-15, -138.9999999999999716 ) ) ;
#20841 = CYLINDRICAL_SURFACE ( 'NONE', #569, 7.500000000000007105 ) ;
#20842 = EDGE_CURVE ( 'NONE', #13331, #6133, #8555, .T. ) ;
#20843 = CYLINDRICAL_SURFACE ( 'NONE', #5344, 2.649999999999971934 ) ;
#20844 = CARTESIAN_POINT ( 'NONE',  ( -6.473970235329672780E-16, -4.862606272033106691, -3.745885042887442395 ) ) ;
#20845 = CARTESIAN_POINT ( 'NONE',  ( -7.922798540899431252, 4.627424769998836673, -8.057412477672047046 ) ) ;
#20846 = ORIENTED_EDGE ( 'NONE', *, *, #17263, .F. ) ;
#20847 = CONTEXT_DEPENDENT_SHAPE_REPRESENTATION ( #3509, #5075 ) ;
#20848 = CARTESIAN_POINT ( 'NONE',  ( -45.00000000000000000, 250.0000000000000000, -5.249999999999956479 ) ) ;
#20849 = EDGE_CURVE ( 'NONE', #16807, #18546, #15879, .T. ) ;
#20850 = DIRECTION ( 'NONE',  ( 0.000000000000000000, 1.000000000000000000, -9.256405414277014607E-16 ) ) ;
#20851 = DIRECTION ( 'NONE',  ( 0.000000000000000000, -1.000000000000000000, 0.000000000000000000 ) ) ;
#20852 = EDGE_LOOP ( 'NONE', ( #15839, #4682, #4378, #17626 ) ) ;
#20853 = AXIS2_PLACEMENT_3D ( 'NONE', #8818, #23549, #13418 ) ;
#20854 = VERTEX_POINT ( 'NONE', #9270 ) ;
#20855 = DIRECTION ( 'NONE',  ( 0.000000000000000000, 0.000000000000000000, 1.000000000000000000 ) ) ;
#20856 = CARTESIAN_POINT ( 'NONE',  ( -282.2000000000010687, -19.99999999999898392, 102.3500000000000227 ) ) ;
#20857 = EDGE_CURVE ( 'NONE', #19306, #18285, #18093, .T. ) ;
#20858 = EDGE_CURVE ( 'NONE', #19820, #19084, #22155, .T. ) ;
#20860 = DIRECTION ( 'NONE',  ( 0.000000000000000000, -3.495664435217746987E-15, 1.000000000000000000 ) ) ;
#20859 = PRODUCT_DEFINITION_SHAPE ( 'NONE', 'NONE',  #23859 ) ;
#20861 = ORIENTED_EDGE ( 'NONE', *, *, #11631, .T. ) ;
#20862 = LINE ( 'NONE', #13546, #20356 ) ;
#20863 = CARTESIAN_POINT ( 'NONE',  ( 45.00000000000000000, 269.9999999999999432, 5.249999999999973355 ) ) ;
#20864 = DIRECTION ( 'NONE',  ( -3.051161311199799893E-31, -1.000000000000000000, 0.000000000000000000 ) ) ;
#20865 = ORIENTED_EDGE ( 'NONE', *, *, #17435, .F. ) ;
#20866 = CARTESIAN_POINT ( 'NONE',  ( 280.6845057130643113, 271.7107452280322377, 148.4314821058792404 ) ) ;
#20867 = DIRECTION ( 'NONE',  ( -1.000000000000000000, -0.000000000000000000, -0.000000000000000000 ) ) ;
#20868 = FACE_BOUND ( 'NONE', #3911, .T. ) ;
#20869 = EDGE_LOOP ( 'NONE', ( #12070, #10288, #12923, #22956 ) ) ;
#20870 = CARTESIAN_POINT ( 'NONE',  ( 282.1999999999999318, 267.7999999999999545, -146.4928932188133786 ) ) ;
#20871 = ITEM_DEFINED_TRANSFORMATION ( 'NONE', 'NONE', #16204,  #11210 ) ;
#20872 = DIRECTION ( 'NONE',  ( 1.000000000000000000, 0.000000000000000000, -0.000000000000000000 ) ) ;
#20873 = CARTESIAN_POINT ( 'NONE',  ( -146.0000000000000853, -784.4690652294805204, 30.00000000000641620 ) ) ;
#20874 = DIRECTION ( 'NONE',  ( -0.000000000000000000, 1.000000000000000000, -3.469446951953613794E-15 ) ) ;
#20875 = UNCERTAINTY_MEASURE_WITH_UNIT (LENGTH_MEASURE( 1.000000000000000082E-05 ), #20792, 'distance_accuracy_value', 'NONE');
#20876 = ORIENTED_EDGE ( 'NONE', *, *, #15584, .T. ) ;
#20877 = EDGE_CURVE ( 'NONE', #1864, #19450, #21148, .T. ) ;
#20878 = ORIENTED_EDGE ( 'NONE', *, *, #9187, .T. ) ;
#20879 = CARTESIAN_POINT ( 'NONE',  ( 24.20041621714725011, -6.482064212728088748, 145.0000119999999697 ) ) ;
#20880 = CYLINDRICAL_SURFACE ( 'NONE', #4037, 2.500000000000000444 ) ;
#20881 = EDGE_CURVE ( 'NONE', #3909, #15625, #10388, .T. ) ;
#20882 = EDGE_CURVE ( 'NONE', #15114, #23044, #3920, .T. ) ;
#20883 = ORIENTED_EDGE ( 'NONE', *, *, #8782, .T. ) ;
#20884 = FACE_OUTER_BOUND ( 'NONE', #4505, .T. ) ;
#20885 = EDGE_CURVE ( 'NONE', #7573, #5160, #12719, .T. ) ;
#20886 = CARTESIAN_POINT ( 'NONE',  ( -126.4560199014029251, 89.63188623867937110, 30.16266818053252052 ) ) ;
#20887 = VERTEX_POINT ( 'NONE', #11089 ) ;
#20888 = CYLINDRICAL_SURFACE ( 'NONE', #13775, 2.649999999999971934 ) ;
#20889 = ORIENTED_EDGE ( 'NONE', *, *, #14805, .T. ) ;
#20890 = DIRECTION ( 'NONE',  ( -6.753181414994864868E-15, 6.753181414994864868E-15, -1.000000000000000000 ) ) ;
#20891 = ORIENTED_EDGE ( 'NONE', *, *, #14599, .T. ) ;
#20892 = EDGE_LOOP ( 'NONE', ( #9519, #16044, #4345, #10305 ) ) ;
#20893 = DIRECTION ( 'NONE',  ( 3.469446951953614682E-16, -1.000000000000000000, 3.483493295888648978E-15 ) ) ;
#20894 = FACE_OUTER_BOUND ( 'NONE', #6692, .T. ) ;
#20895 = DIRECTION ( 'NONE',  ( 0.000000000000000000, -1.000000000000000000, 0.000000000000000000 ) ) ;
#20896 = PLANE ( 'NONE',  #1519 ) ;
#20897 = FACE_OUTER_BOUND ( 'NONE', #22947, .T. ) ;
#20898 = ORIENTED_EDGE ( 'NONE', *, *, #4252, .T. ) ;
#20899 = CARTESIAN_POINT ( 'NONE',  ( -2.387978478801491278, -7.281554020289322970, -7.069802615102039667 ) ) ;
#20900 = PRODUCT_DEFINITION_SHAPE ( 'NONE', 'NONE',  #23882 ) ;
#20901 = ORIENTED_EDGE ( 'NONE', *, *, #19832, .F. ) ;
#20902 = CARTESIAN_POINT ( 'NONE',  ( 10.40000000000000036, 6.123233995736768255E-16, -5.000000000000001776 ) ) ;
#20903 = FACE_OUTER_BOUND ( 'NONE', #14066, .T. ) ;
#20904 = AXIS2_PLACEMENT_3D ( 'NONE', #7748, #499, #4095 ) ;
#20905 = ORIENTED_EDGE ( 'NONE', *, *, #6095, .T. ) ;
#20906 = ADVANCED_FACE ( 'NONE', ( #12681, #9382, #20116, #7436, #7553 ), #18297, .F. ) ;
#20907 = DIRECTION ( 'NONE',  ( 1.000000000000000000, 0.000000000000000000, 0.000000000000000000 ) ) ;
#20908 = ORIENTED_EDGE ( 'NONE', *, *, #6969, .F. ) ;
#20909 = LINE ( 'NONE', #11772, #8677 ) ;
#20910 = CARTESIAN_POINT ( 'NONE',  ( 1.567478505476134606E-15, 4.618802153517012066, -3.433295621305382905 ) ) ;
#20911 = VERTEX_POINT ( 'NONE', #9023 ) ;
#20912 = CARTESIAN_POINT ( 'NONE',  ( -281.4928932188135491, 267.7999999999999545, 150.1999999999999886 ) ) ;
#20913 = DIRECTION ( 'NONE',  ( 0.000000000000000000, -2.618450529776326854E-15, -1.000000000000000000 ) ) ;
#20914 = ORIENTED_EDGE ( 'NONE', *, *, #12148, .F. ) ;
#20915 = CARTESIAN_POINT ( 'NONE',  ( -44.99999999999997868, -52.79999999999938609, 140.0000000000001421 ) ) ;
#20916 = DIRECTION ( 'NONE',  ( -0.000000000000000000, 1.000000000000000000, -3.469446951953613794E-15 ) ) ;
#20917 = LINE ( 'NONE', #22484, #19242 ) ;
#20918 = AXIS2_PLACEMENT_3D ( 'NONE', #230, #9529, #13420 ) ;
#20919 = CARTESIAN_POINT ( 'NONE',  ( 10.00000000000000000, 0.000000000000000000, -50.00000000000000000 ) ) ;
#20920 = ORIENTED_EDGE ( 'NONE', *, *, #14807, .F. ) ;
#20921 = CARTESIAN_POINT ( 'NONE',  ( -280.6220388411722411, 269.5350371479513569, -146.3333820183295302 ) ) ;
#20923 = EDGE_LOOP ( 'NONE', ( #22226, #3786, #14091, #8895 ) ) ;
#20922 = EDGE_LOOP ( 'NONE', ( #7622, #1723, #1193, #5171 ) ) ;
#20924 = DIRECTION ( 'NONE',  ( -6.982962677686266711E-15, 9.837870180509810443E-29, -1.000000000000000000 ) ) ;
#20925 = DIRECTION ( 'NONE',  ( 0.000000000000000000, 1.000000000000000000, 0.000000000000000000 ) ) ;
#20926 = DIRECTION ( 'NONE',  ( -0.000000000000000000, 0.000000000000000000, -1.000000000000000000 ) ) ;
#20927 = EDGE_CURVE ( 'NONE', #2779, #21906, #18410, .T. ) ;
#20928 = CARTESIAN_POINT ( 'NONE',  ( 280.2880230824754335, 269.9999999999999432, 145.1244266708879707 ) ) ;
#20929 = EDGE_CURVE ( 'NONE', #20119, #907, #2652, .T. ) ;
#20930 = DIRECTION ( 'NONE',  ( 0.000000000000000000, 0.000000000000000000, 1.000000000000000000 ) ) ;
#20931 = ORIENTED_EDGE ( 'NONE', *, *, #215, .F. ) ;
#20932 = EDGE_CURVE ( 'NONE', #11056, #4336, #7189, .T. ) ;
#20933 = AXIS2_PLACEMENT_3D ( 'NONE', #19792, #21368, #4952 ) ;
#20934 = APPLICATION_CONTEXT ( 'automotive_design' ) ;
#20935 = FACE_OUTER_BOUND ( 'NONE', #565, .T. ) ;
#20936 = CARTESIAN_POINT ( 'NONE',  ( 0.000000000000000000, 0.000000000000000000, -100.0000000000000000 ) ) ;
#20937 = LINE ( 'NONE', #777, #3 ) ;
#20938 = EDGE_CURVE ( 'NONE', #5337, #22099, #1643, .T. ) ;
#20939 = EDGE_CURVE ( 'NONE', #22438, #11911, #7644, .T. ) ;
#20940 = EDGE_LOOP ( 'NONE', ( #14594, #12513, #22171, #10927 ) ) ;
#20941 = DIRECTION ( 'NONE',  ( 0.000000000000000000, -2.618450529776313049E-15, -1.000000000000000000 ) ) ;
#20942 = ORIENTED_EDGE ( 'NONE', *, *, #1344, .T. ) ;
#20943 = DIRECTION ( 'NONE',  ( 1.000000000000000000, 0.000000000000000000, 0.000000000000000000 ) ) ;
#20944 = DIRECTION ( 'NONE',  ( 0.000000000000000000, 0.000000000000000000, 1.000000000000000000 ) ) ;
#20945 = B_SPLINE_CURVE_WITH_KNOTS ( 'NONE', 3,
 ( #13986, #17452, #21193, #8037, #4762, #6336, #11936, #9859, #19249, #17557, #13519, #4291, #17341, #6226, #1007, #13634, #4656, #13862, #15539, #12069, #20947, #7912, #21309, #791, #4403, #19364, #2467, #891, #11812, #8274, #2822, #8169, #22864, #13745 ),
 .UNSPECIFIED., .F., .F.,
 ( 4, 2, 2, 2, 2, 2, 2, 2, 2, 2, 2, 2, 2, 2, 2, 2, 4 ),
 ( 0.2500000000000000000, 0.2812500000000000000, 0.3125000000000000000, 0.3437500000000000000, 0.3750000000000000000, 0.4062500000000000000, 0.4375000000000000000, 0.4687500000000000000, 0.5000000000000000000, 0.5312500000000000000, 0.5625000000000000000, 0.5937500000000000000, 0.6250000000000000000, 0.6562500000000000000, 0.6875000000000000000, 0.7187500000000000000, 0.7500000000000000000 ),
 .UNSPECIFIED. ) ;
#20946 = ORIENTED_EDGE ( 'NONE', *, *, #13058, .T. ) ;
#20947 = CARTESIAN_POINT ( 'NONE',  ( -8.050072859967690064, 23.72540897006225791, -145.0000000000000000 ) ) ;
#20948 = VERTEX_POINT ( 'NONE', #7322 ) ;
#20949 = CARTESIAN_POINT ( 'NONE',  ( 146.4449999999997942, -801.0618695410399823, 30.00000000000641975 ) ) ;
#20950 = CARTESIAN_POINT ( 'NONE',  ( -0.3198814748697807464, -4.434118497892185040, -0.3507732604232532969 ) ) ;
#20951 = CARTESIAN_POINT ( 'NONE',  ( -31.74999999999995737, 0.000000000000000000, 0.000000000000000000 ) ) ;
#20952 = ADVANCED_FACE ( 'NONE', ( #3562, #7081 ), #16383, .T. ) ;
#20953 = VECTOR ( 'NONE', #15026, 1000.000000000000000 ) ;
#20954 = DIRECTION ( 'NONE',  ( -0.000000000000000000, -0.000000000000000000, 1.000000000000000000 ) ) ;
#20955 = DIRECTION ( 'NONE',  ( 1.000000000000000000, -0.000000000000000000, 6.982962677686266711E-15 ) ) ;
#20956 = DIRECTION ( 'NONE',  ( -0.000000000000000000, -0.000000000000000000, 1.000000000000000000 ) ) ;
#20957 = CARTESIAN_POINT ( 'NONE',  ( -40.00000000000000000, 100.0000000000000000, 147.2000000000005855 ) ) ;
#20958 = AXIS2_PLACEMENT_3D ( 'NONE', #20957, #15900, #23121 ) ;
#20959 = VERTEX_POINT ( 'NONE', #21808 ) ;
#20960 =( LENGTH_UNIT ( ) NAMED_UNIT ( * ) SI_UNIT ( .MILLI., .METRE. ) );
#20961 = FACE_OUTER_BOUND ( 'NONE', #22929, .T. ) ;
#20962 = CARTESIAN_POINT ( 'NONE',  ( -121.5574576620399654, 79.04925354955206274, -2.775557561562891351E-14 ) ) ;
#20963 = VERTEX_POINT ( 'NONE', #19994 ) ;
#20964 = ORIENTED_EDGE ( 'NONE', *, *, #22470, .F. ) ;
#20965 = DIRECTION ( 'NONE',  ( 1.000000000000000000, 0.000000000000000000, -0.000000000000000000 ) ) ;
#20966 = DIRECTION ( 'NONE',  ( -1.000000000000000000, -0.000000000000000000, -0.000000000000000000 ) ) ;
#20967 = FACE_OUTER_BOUND ( 'NONE', #20170, .T. ) ;
#20968 = CIRCLE ( 'NONE', #5539, 145.0000000000000284 ) ;
#20969 = CIRCLE ( 'NONE', #22107, 5.249999999999949374 ) ;
#20970 = ORIENTED_EDGE ( 'NONE', *, *, #17571, .F. ) ;
#20971 = CARTESIAN_POINT ( 'NONE',  ( -194.7500000000004547, -494.4690652294794404, -27.49999999999322498 ) ) ;
#20972 = DIRECTION ( 'NONE',  ( 0.000000000000000000, -3.491481338843133355E-15, 1.000000000000000000 ) ) ;
#20973 = ADVANCED_FACE ( 'NONE', ( #23735 ), #1870, .T. ) ;
#20974 = DIRECTION ( 'NONE',  ( 1.000000000000000000, -0.000000000000000000, -0.000000000000000000 ) ) ;
#20975 = EDGE_CURVE ( 'NONE', #5337, #17412, #16168, .T. ) ;
#20976 = ORIENTED_EDGE ( 'NONE', *, *, #3968, .F. ) ;
#20977 = CARTESIAN_POINT ( 'NONE',  ( 0.000000000000000000, -1000.000000000000000, 138.9999999999999716 ) ) ;
#20978 = CARTESIAN_POINT ( 'NONE',  ( 45.00000000000000000, 269.9999999999999432, -5.249999999999973355 ) ) ;
#20979 = EDGE_CURVE ( 'NONE', #18017, #10087, #21548, .T. ) ;
#20980 = CARTESIAN_POINT ( 'NONE',  ( 110.0000000000000000, -74.99999999999998579, 3.000000000000000000 ) ) ;
#20981 = ORIENTED_EDGE ( 'NONE', *, *, #11417, .T. ) ;
#20982 = CARTESIAN_POINT ( 'NONE',  ( 281.4928932188134354, 267.8000000000000114, -147.1999999999999318 ) ) ;
#20983 = ADVANCED_FACE ( 'NONE', ( #22403 ), #18898, .F. ) ;
#20984 = ITEM_DEFINED_TRANSFORMATION ( 'NONE', 'NONE', #1538,  #11210 ) ;
#20985 = CARTESIAN_POINT ( 'NONE',  ( 0.000000000000000000, 1.178949249685218081, 2.041999999999998483 ) ) ;
#20986 = EDGE_CURVE ( 'NONE', #8126, #9666, #15770, .T. ) ;
#20987 =( REPRESENTATION_RELATIONSHIP ('NONE','NONE', #10127, #6236 ) REPRESENTATION_RELATIONSHIP_WITH_TRANSFORMATION ( #11052 )SHAPE_REPRESENTATION_RELATIONSHIP( ) );
#20988 = ADVANCED_FACE ( 'NONE', ( #557 ), #20843, .F. ) ;
#20989 = DIRECTION ( 'NONE',  ( 0.000000000000000000, -1.000000000000000000, 0.000000000000000000 ) ) ;
#20990 = LINE ( 'NONE', #22668, #19763 ) ;
#20991 =( GEOMETRIC_REPRESENTATION_CONTEXT ( 3 ) GLOBAL_UNCERTAINTY_ASSIGNED_CONTEXT ( ( #2507 ) ) GLOBAL_UNIT_ASSIGNED_CONTEXT ( ( #10014, #15799, #19152 ) ) REPRESENTATION_CONTEXT ( 'NONE', 'WORKASPACE' ) );
#20992 = EDGE_LOOP ( 'NONE', ( #14915, #2586, #23024, #15701 ) ) ;
#20993 = AXIS2_PLACEMENT_3D ( 'NONE', #21888, #16253, #5361 ) ;
#20994 = ORIENTED_EDGE ( 'NONE', *, *, #20532, .T. ) ;
#20995 = DIRECTION ( 'NONE',  ( -0.000000000000000000, 1.000000000000000000, -0.000000000000000000 ) ) ;
#20996 = CARTESIAN_POINT ( 'NONE',  ( -287.4000000000014552, -127.0000000000000568, -146.4928932188134070 ) ) ;
#20997 = AXIS2_PLACEMENT_3D ( 'NONE', #22554, #2517, #14985 ) ;
#20998 = ORIENTED_EDGE ( 'NONE', *, *, #21833, .F. ) ;
#20999 = FACE_OUTER_BOUND ( 'NONE', #8940, .T. ) ;
#21000 = CARTESIAN_POINT ( 'NONE',  ( 0.000000000000000000, 0.000000000000000000, -150.2000000000008981 ) ) ;
#21002 = ORIENTED_EDGE ( 'NONE', *, *, #10358, .F. ) ;
#21001 = VECTOR ( 'NONE', #22854, 1000.000000000000000 ) ;
#21003 = CARTESIAN_POINT ( 'NONE',  ( 312.2000000000013529, -129.2000000000000455, -146.4928932188134070 ) ) ;
#21004 = VERTEX_POINT ( 'NONE', #13642 ) ;
#21005 = CARTESIAN_POINT ( 'NONE',  ( -4.000000000000000888, -2.309401076758512694, -3.504269196027526512 ) ) ;
#21006 = LINE ( 'NONE', #10275, #14439 ) ;
#21007 = EDGE_LOOP ( 'NONE', ( #10460, #10343, #19842, #18715 ) ) ;
#21008 = ORIENTED_EDGE ( 'NONE', *, *, #6136, .T. ) ;
#21009 = CARTESIAN_POINT ( 'NONE',  ( 4.197393957002303999, 0.8151795401431359833, -3.503767560748935139 ) ) ;
#21010 = VECTOR ( 'NONE', #5907, 1000.000000000000000 ) ;
#21011 = AXIS2_PLACEMENT_3D ( 'NONE', #22715, #4364, #1851 ) ;
#21012 = CARTESIAN_POINT ( 'NONE',  ( -44.99999999999995026, -56.79999999999968452, 105.0000000000002132 ) ) ;
#21013 = ADVANCED_FACE ( 'NONE', ( #2591 ), #2109, .F. ) ;
#21014 = EDGE_CURVE ( 'NONE', #12275, #4892, #22515, .T. ) ;
#21015 = CARTESIAN_POINT ( 'NONE',  ( 7.922281120364393914, -4.573931137438282057, -8.047472243342932430 ) ) ;
#21016 = CARTESIAN_POINT ( 'NONE',  ( 5.000000000000004441, 0.000000000000000000, 4.250000000000000000 ) ) ;
#21017 = ORIENTED_EDGE ( 'NONE', *, *, #15460, .T. ) ;
#21018 = DIRECTION ( 'NONE',  ( 0.000000000000000000, -1.000000000000000000, -1.110223024625156540E-16 ) ) ;
#21019 = VECTOR ( 'NONE', #2986, 1000.000000000000000 ) ;
#21020 = ORIENTED_EDGE ( 'NONE', *, *, #8285, .F. ) ;
#21021 = CARTESIAN_POINT ( 'NONE',  ( 0.000000000000000000, 2.357898499370433054, -1.951563910473907981E-15 ) ) ;
#21022 = VECTOR ( 'NONE', #21613, 1000.000000000000000 ) ;
#21023 = EDGE_LOOP ( 'NONE', ( #9404, #16555, #4772, #12690 ) ) ;
#21024 = CARTESIAN_POINT ( 'NONE',  ( -6.487492490819623647, -24.19938668346784638, -145.0000000000000000 ) ) ;
#21025 = ORIENTED_EDGE ( 'NONE', *, *, #12899, .F. ) ;
#21026 = CARTESIAN_POINT ( 'NONE',  ( 7.500000000000000888, 1.443375672974060109, -7.063244554130000630 ) ) ;
#21027 = LINE ( 'NONE', #11896, #6765 ) ;
#21028 = ORIENTED_EDGE ( 'NONE', *, *, #21226, .F. ) ;
#21029 = AXIS2_PLACEMENT_3D ( 'NONE', #21382, #744, #6297 ) ;
#21030 = CARTESIAN_POINT ( 'NONE',  ( -280.8708543776413080, 270.9956429438695409, 149.1582675804705218 ) ) ;
#21031 = FILL_AREA_STYLE ('',( #11409 ) ) ;
#21032 = VERTEX_POINT ( 'NONE', #9865 ) ;
#21033 = UNCERTAINTY_MEASURE_WITH_UNIT (LENGTH_MEASURE( 1.000000000000000082E-05 ), #2083, 'distance_accuracy_value', 'NONE');
#21034 = CARTESIAN_POINT ( 'NONE',  ( -93.00000000000000000, 3.053113317719180486E-13, 129.9038105676659711 ) ) ;
#21035 = FACE_OUTER_BOUND ( 'NONE', #20309, .T. ) ;
#21036 = DIRECTION ( 'NONE',  ( 0.000000000000000000, 0.000000000000000000, -1.000000000000000000 ) ) ;
#21037 = VECTOR ( 'NONE', #11693, 1000.000000000000000 ) ;
#21038 = VECTOR ( 'NONE', #7728, 1000.000000000000000 ) ;
#21039 = CARTESIAN_POINT ( 'NONE',  ( -0.2727178028658734932, 0.000000000000000000, 0.000000000000000000 ) ) ;
#21040 = EDGE_LOOP ( 'NONE', ( #8514, #14415, #11114, #12998, #13652, #1563 ) ) ;
#21041 = DIRECTION ( 'NONE',  ( -1.000000000000000000, -0.000000000000000000, -0.000000000000000000 ) ) ;
#21042 =( NAMED_UNIT ( * ) PLANE_ANGLE_UNIT ( ) SI_UNIT ( $, .RADIAN. ) );
#21043 = PRODUCT_DEFINITION_SHAPE ( 'NONE', 'NONE',  #23848 ) ;
#21045 = ORIENTED_EDGE ( 'NONE', *, *, #4999, .F. ) ;
#21044 = ORIENTED_EDGE ( 'NONE', *, *, #20772, .T. ) ;
#21046 = CARTESIAN_POINT ( 'NONE',  ( 142.1569981022710465, 83.57863297847711692, 30.00000000000653699 ) ) ;
#21047 = CARTESIAN_POINT ( 'NONE',  ( 51.87806360044629628, 135.4018704341563364, 90.00000000000000000 ) ) ;
#21048 = VECTOR ( 'NONE', #18289, 1000.000000000000000 ) ;
#21049 = DIRECTION ( 'NONE',  ( 0.000000000000000000, -1.000000000000000000, 0.000000000000000000 ) ) ;
#21050 = CARTESIAN_POINT ( 'NONE',  ( -31.74999999999995737, 0.000000000000000000, 0.000000000000000000 ) ) ;
#21051 = CIRCLE ( 'NONE', #11049, 0.3000000000000051514 ) ;
#21052 = DIRECTION ( 'NONE',  ( -1.000000000000000000, 0.000000000000000000, 0.000000000000000000 ) ) ;
#21053 = ORIENTED_EDGE ( 'NONE', *, *, #12405, .T. ) ;
#21054 = VECTOR ( 'NONE', #15509, 1000.000000000000000 ) ;
#21055 = DIRECTION ( 'NONE',  ( -0.000000000000000000, -0.000000000000000000, 1.000000000000000000 ) ) ;
#21056 = CARTESIAN_POINT ( 'NONE',  ( 0.2500000000000002220, 4.898587196589412829E-16, -3.999999999999979128 ) ) ;
#21057 = CARTESIAN_POINT ( 'NONE',  ( 123.0250976530554539, -1094.285891978964173, 30.80845853161007497 ) ) ;
#21058 = CONTEXT_DEPENDENT_SHAPE_REPRESENTATION ( #1038, #17986 ) ;
#21059 = EDGE_CURVE ( 'NONE', #10116, #16800, #17352, .T. ) ;
#21060 = ORIENTED_EDGE ( 'NONE', *, *, #23610, .T. ) ;
#21061 = CARTESIAN_POINT ( 'NONE',  ( -51.87806360044717735, -135.4018704341559669, -2.775557561562891351E-14 ) ) ;
#21062 = VERTEX_POINT ( 'NONE', #17221 ) ;
#21063 = CARTESIAN_POINT ( 'NONE',  ( -105.0000000000000142, 30.00000000000001421, 3.000000000000001332 ) ) ;
#21064 = DIRECTION ( 'NONE',  ( 0.000000000000000000, 1.334402673828305746E-15, -1.000000000000000000 ) ) ;
#21065 = ORIENTED_EDGE ( 'NONE', *, *, #7494, .F. ) ;
#21066 = VECTOR ( 'NONE', #5377, 1000.000000000000000 ) ;
#21067 = CARTESIAN_POINT ( 'NONE',  ( 20.00000000000000000, -1000.000000000000000, -125.0000000000001137 ) ) ;
#21068 = VERTEX_POINT ( 'NONE', #4528 ) ;
#21069 = CARTESIAN_POINT ( 'NONE',  ( 2.500000000000000000, -1.178949249685213863, 2.042000000000002924 ) ) ;
#21070 = FACE_OUTER_BOUND ( 'NONE', #1348, .T. ) ;
#21071 = EDGE_CURVE ( 'NONE', #13072, #17463, #11960, .T. ) ;
#21072 = CARTESIAN_POINT ( 'NONE',  ( 2.500000000000000000, -1.178949249685213863, 2.042000000000001148 ) ) ;
#21073 = CARTESIAN_POINT ( 'NONE',  ( 5.000000000000000000, 4.685197434473814759, -5.637851296924623057E-15 ) ) ;
#21074 = DIRECTION ( 'NONE',  ( -0.000000000000000000, -0.000000000000000000, 1.000000000000000000 ) ) ;
#21075 = EDGE_CURVE ( 'NONE', #22831, #18827, #1495, .T. ) ;
#21076 = DIRECTION ( 'NONE',  ( -1.350636282998972974E-14, 0.000000000000000000, -1.000000000000000000 ) ) ;
#21077 = ORIENTED_EDGE ( 'NONE', *, *, #23030, .F. ) ;
#21078 = DIRECTION ( 'NONE',  ( -1.000000000000000000, 0.000000000000000000, 0.000000000000000000 ) ) ;
#21079 = CARTESIAN_POINT ( 'NONE',  ( -4.000000000000000000, -2.512220745329312610, -3.469390707569719901 ) ) ;
#21080 = ADVANCED_FACE ( 'NONE', ( #15183 ), #3017, .F. ) ;
#21081 = VERTEX_POINT ( 'NONE', #671 ) ;
#21082 = ORIENTED_EDGE ( 'NONE', *, *, #13505, .F. ) ;
#21083 = FACE_OUTER_BOUND ( 'NONE', #23785, .T. ) ;
#21084 = CYLINDRICAL_SURFACE ( 'NONE', #6484, 2.649999999999971934 ) ;
#21085 = AXIS2_PLACEMENT_3D ( 'NONE', #16585, #23802, #7146 ) ;
#21086 = ORIENTED_EDGE ( 'NONE', *, *, #8611, .F. ) ;
#21087 = CYLINDRICAL_SURFACE ( 'NONE', #8297, 2.500000000000002220 ) ;
#21088 = CARTESIAN_POINT ( 'NONE',  ( -44.80746418436648071, -137.9031948627975908, 90.00000000000000000 ) ) ;
#21089 = DIRECTION ( 'NONE',  ( 1.000000000000000000, 0.000000000000000000, 0.000000000000000000 ) ) ;
#21090 = CARTESIAN_POINT ( 'NONE',  ( -3.680118525130244400, 2.494084732383327285, -0.3507732604232449702 ) ) ;
#21091 = ORIENTED_EDGE ( 'NONE', *, *, #14644, .T. ) ;
#21092 = DIRECTION ( 'NONE',  ( 0.000000000000000000, -1.000000000000000000, 0.000000000000000000 ) ) ;
#21093 = DIRECTION ( 'NONE',  ( 0.000000000000000000, 0.5000000000000009992, 0.8660254037844380415 ) ) ;
#21094 = FACE_OUTER_BOUND ( 'NONE', #18416, .T. ) ;
#21095 = EDGE_LOOP ( 'NONE', ( #3176, #8218, #21821, #3600 ) ) ;
#21096 = AXIS2_PLACEMENT_3D ( 'NONE', #4955, #15718, #12493 ) ;
#21097 = DIRECTION ( 'NONE',  ( -0.000000000000000000, 1.000000000000000000, 0.000000000000000000 ) ) ;
#21098 = B_SPLINE_CURVE_WITH_KNOTS ( 'NONE', 3,
 ( #13017, #3657, #70, #7421, #14806, #22137, #20323, #9817, #3781, #7993 ),
 .UNSPECIFIED., .F., .F.,
 ( 4, 2, 2, 2, 4 ),
 ( 0.01051144076094935251, 0.01162027323572611265, 0.01272910571050287452, 0.01383793818527963640, 0.01494677066005639827 ),
 .UNSPECIFIED. ) ;
#21099 = PRODUCT_CONTEXT ( 'NONE', #8923, 'mechanical' ) ;
#21100 = DIRECTION ( 'NONE',  ( 4.625929269271498733E-16, 0.000000000000000000, 1.000000000000000000 ) ) ;
#21101 = VECTOR ( 'NONE', #12224, 1000.000000000000000 ) ;
#21102 = PLANE ( 'NONE',  #13497 ) ;
#21103 = CARTESIAN_POINT ( 'NONE',  ( -3.750000000000007105, -6.495190528383289141, 0.000000000000000000 ) ) ;
#21104 = ADVANCED_FACE ( 'NONE', ( #797 ), #15546, .T. ) ;
#21105 = ORIENTED_EDGE ( 'NONE', *, *, #18555, .T. ) ;
#21106 = ORIENTED_EDGE ( 'NONE', *, *, #3009, .T. ) ;
#21107 = CARTESIAN_POINT ( 'NONE',  ( -280.2481149223241346, 269.9433523009093392, -145.5743436287470161 ) ) ;
#21108 = LINE ( 'NONE', #4567, #23116 ) ;
#21109 = EDGE_CURVE ( 'NONE', #21209, #18124, #21911, .T. ) ;
#21110 = ORIENTED_EDGE ( 'NONE', *, *, #8229, .F. ) ;
#21111 = ADVANCED_FACE ( 'NONE', ( #13749 ), #6342, .T. ) ;
#21112 = AXIS2_PLACEMENT_3D ( 'NONE', #22050, #19886, #20345 ) ;
#21113 = ORIENTED_EDGE ( 'NONE', *, *, #21802, .F. ) ;
#21114 = FACE_OUTER_BOUND ( 'NONE', #13192, .T. ) ;
#21115 = EDGE_CURVE ( 'NONE', #15682, #4339, #7264, .T. ) ;
#21116 = CARTESIAN_POINT ( 'NONE',  ( 80.00000000000000000, -61.99999999999998579, 3.000000000000000000 ) ) ;
#21117 = PRODUCT_RELATED_PRODUCT_CATEGORY ( 'part', '', ( #10385 ) ) ;
#21118 = EDGE_LOOP ( 'NONE', ( #10628, #13486, #12496, #22813, #6192 ) ) ;
#21119 = AXIS2_PLACEMENT_3D ( 'NONE', #48, #21656, #3523 ) ;
#21120 = DIRECTION ( 'NONE',  ( 1.000000000000000000, 0.000000000000000000, 0.000000000000000000 ) ) ;
#21121 = AXIS2_PLACEMENT_3D ( 'NONE', #22347, #3978, #9555 ) ;
#21122 = AXIS2_PLACEMENT_3D ( 'NONE', #23529, #11654, #732 ) ;
#21123 = ORIENTED_EDGE ( 'NONE', *, *, #16358, .F. ) ;
#21124 = LINE ( 'NONE', #17497, #7927 ) ;
#21125 = DIRECTION ( 'NONE',  ( 1.000000000000000000, 3.736327486719275871E-16, -1.296299001029869881E-30 ) ) ;
#21126 = EDGE_LOOP ( 'NONE', ( #10401, #1265, #22687, #9045 ) ) ;
#21127 = ORIENTED_EDGE ( 'NONE', *, *, #23030, .T. ) ;
#21128 = DIRECTION ( 'NONE',  ( 5.135813185032629306E-32, -1.850371707708594366E-15, -1.000000000000000000 ) ) ;
#21129 = CARTESIAN_POINT ( 'NONE',  ( 3.436319922986518449, -2.634841920959471562, -3.531542292954761741 ) ) ;
#21130 = AXIS2_PLACEMENT_3D ( 'NONE', #11706, #9633, #20850 ) ;
#21131 = DIRECTION ( 'NONE',  ( 1.000000000000000000, 0.000000000000000000, -0.000000000000000000 ) ) ;
#21132 = CYLINDRICAL_SURFACE ( 'NONE', #23505, 5.249999999999942268 ) ;
#21133 = EDGE_LOOP ( 'NONE', ( #966, #5706, #2132 ) ) ;
#21134 = VECTOR ( 'NONE', #21457, 1000.000000000000000 ) ;
#21135 = CARTESIAN_POINT ( 'NONE',  ( -3.295171437451516638, -7.213553046160524396, -7.590212325761481971 ) ) ;
#21136 = CIRCLE ( 'NONE', #13851, 23.97500000000000142 ) ;
#21137 = CIRCLE ( 'NONE', #2232, 25.00000000000000000 ) ;
#21138 = VERTEX_POINT ( 'NONE', #15304 ) ;
#21139 = VERTEX_POINT ( 'NONE', #6106 ) ;
#21140 = CARTESIAN_POINT ( 'NONE',  ( -22.46856765562321812, -11.08409875796190214, -145.0000000000000000 ) ) ;
#21141 = ADVANCED_FACE ( 'NONE', ( #13527 ), #8763, .T. ) ;
#21142 = VERTEX_POINT ( 'NONE', #21424 ) ;
#21144 = EDGE_CURVE ( 'NONE', #846, #15958, #3072, .T. ) ;
#21143 = CARTESIAN_POINT ( 'NONE',  ( 45.00000000000000000, 269.9999999999999432, 0.000000000000000000 ) ) ;
#21145 = PLANE ( 'NONE',  #21029 ) ;
#21146 = VERTEX_POINT ( 'NONE', #1262 ) ;
#21147 = COLOUR_RGB ( '',0.8941176470588234615, 0.8941176470588234615, 0.8941176470588234615 ) ;
#21148 = CIRCLE ( 'NONE', #3399, 5.000000000000000888 ) ;
#21149 = CARTESIAN_POINT ( 'NONE',  ( -280.0000000000000568, 269.9696999999999889, 145.0000000000000284 ) ) ;
#21150 = CYLINDRICAL_SURFACE ( 'NONE', #4427, 7.500000000000007105 ) ;
#21151 = AXIS2_PLACEMENT_3D ( 'NONE', #6520, #16820, #11536 ) ;
#21152 = ORIENTED_EDGE ( 'NONE', *, *, #18850, .T. ) ;
#21153 = AXIS2_PLACEMENT_3D ( 'NONE', #8727, #16091, #12623 ) ;
#21154 = DIRECTION ( 'NONE',  ( 1.000000000000000000, 0.000000000000000000, 0.000000000000000000 ) ) ;
#21155 = CARTESIAN_POINT ( 'NONE',  ( -24.83992656739931704, -996.7332239287533184, -145.0000000000001421 ) ) ;
#21156 = AXIS2_PLACEMENT_3D ( 'NONE', #10863, #10728, #6968 ) ;
#21157 = CARTESIAN_POINT ( 'NONE',  ( 10.40000000000000036, 0.000000000000000000, 0.000000000000000000 ) ) ;
#21158 = CARTESIAN_POINT ( 'NONE',  ( 0.000000000000000000, 0.000000000000000000, 35.00000000000000000 ) ) ;
#21159 = ORIENTED_EDGE ( 'NONE', *, *, #22133, .T. ) ;
#21160 = DIRECTION ( 'NONE',  ( 0.000000000000000000, 0.000000000000000000, -1.000000000000000000 ) ) ;
#21162 = ORIENTED_EDGE ( 'NONE', *, *, #5095, .T. ) ;
#21161 = ORIENTED_EDGE ( 'NONE', *, *, #904, .F. ) ;
#21163 = VECTOR ( 'NONE', #7671, 1000.000000000000000 ) ;
#21164 = DIRECTION ( 'NONE',  ( 1.000000000000000000, 0.000000000000000000, 0.000000000000000000 ) ) ;
#21166 = AXIS2_PLACEMENT_3D ( 'NONE', #20471, #13036, #11333 ) ;
#21165 = COLOUR_RGB ( '',0.8941176470588234615, 0.8941176470588234615, 0.8941176470588234615 ) ;
#21168 = CARTESIAN_POINT ( 'NONE',  ( 7.499999999999999112, 4.652409454067514716, -7.929128589908465585 ) ) ;
#21167 = CIRCLE ( 'NONE', #18094, 4.000000000000000000 ) ;
#21169 = DIRECTION ( 'NONE',  ( 0.000000000000000000, -3.491481338843133355E-15, 1.000000000000000000 ) ) ;
#21170 = CIRCLE ( 'NONE', #17706, 2.499999999999998668 ) ;
#21171 = AXIS2_PLACEMENT_3D ( 'NONE', #7765, #269, #20913 ) ;
#21172 = VECTOR ( 'NONE', #17371, 1000.000000000000000 ) ;
#21173 = DIRECTION ( 'NONE',  ( 0.000000000000000000, -1.000000000000000000, 0.000000000000000000 ) ) ;
#21174 = FACE_OUTER_BOUND ( 'NONE', #21184, .T. ) ;
#21175 = CARTESIAN_POINT ( 'NONE',  ( -281.9223300543794721, 268.9079617568158938, -145.9952621458756141 ) ) ;
#21176 = EDGE_CURVE ( 'NONE', #4246, #8364, #21549, .T. ) ;
#21177 = ORIENTED_EDGE ( 'NONE', *, *, #3202, .T. ) ;
#21178 = VECTOR ( 'NONE', #15911, 1000.000000000000000 ) ;
#21179 = DIRECTION ( 'NONE',  ( 0.000000000000000000, -3.469446951953613794E-15, -1.000000000000000000 ) ) ;
#21180 = EDGE_CURVE ( 'NONE', #13741, #12953, #16536, .T. ) ;
#21181 = DIRECTION ( 'NONE',  ( 0.000000000000000000, -0.000000000000000000, -1.000000000000000000 ) ) ;
#21182 = FILL_AREA_STYLE_COLOUR ( '', #8866 ) ;
#21183 = ITEM_DEFINED_TRANSFORMATION ( 'NONE', 'NONE', #3061,  #11210 ) ;
#21184 = EDGE_LOOP ( 'NONE', ( #10938, #7397, #7043, #2941 ) ) ;
#21185 = DIRECTION ( 'NONE',  ( 0.6964005597823107463, -0.7176533009294140397, 6.982962677686265922E-15 ) ) ;
#21186 = ORIENTED_EDGE ( 'NONE', *, *, #20157, .T. ) ;
#21187 = PLANE ( 'NONE',  #20417 ) ;
#21188 = LINE ( 'NONE', #15537, #6377 ) ;
#21190 = CIRCLE ( 'NONE', #6914, 2.649999999999985700 ) ;
#21189 = PRESENTATION_LAYER_ASSIGNMENT (  '', '', ( #1113 ) ) ;
#21191 = EDGE_LOOP ( 'NONE', ( #23192, #15969, #3256, #5690, #17652 ) ) ;
#21192 = VECTOR ( 'NONE', #3267, 1000.000000000000000 ) ;
#21193 = CARTESIAN_POINT ( 'NONE',  ( 24.84002319582486606, 3.266795291537505808, -145.0000000000000284 ) ) ;
#21194 = CONICAL_SURFACE ( 'NONE', #3041, 2.055000000000001492, 0.7853981633974633780 ) ;
#21195 = ORIENTED_EDGE ( 'NONE', *, *, #8341, .F. ) ;
#21196 = CONICAL_SURFACE ( 'NONE', #16955, 2.055000000000001492, 0.7853981633974633780 ) ;
#21197 = VECTOR ( 'NONE', #8263, 1000.000000000000000 ) ;
#21198 = CIRCLE ( 'NONE', #6545, 2.041999999999999815 ) ;
#21199 = DIRECTION ( 'NONE',  ( -0.000000000000000000, 1.000000000000000000, -3.469446951953613794E-15 ) ) ;
#21200 = CARTESIAN_POINT ( 'NONE',  ( -40.33333333333332860, -89.99999999999997158, 3.000000000000000000 ) ) ;
#21201 = CARTESIAN_POINT ( 'NONE',  ( 100.0000000000000000, 270.0000000000000000, -144.9999999999999716 ) ) ;
#21202 = DIRECTION ( 'NONE',  ( -0.7071067811865254793, 0.000000000000000000, 0.7071067811865695552 ) ) ;
#21203 = DIRECTION ( 'NONE',  ( 1.000000000000000000, 0.000000000000000000, -0.000000000000000000 ) ) ;
#21204 = ORIENTED_EDGE ( 'NONE', *, *, #18745, .T. ) ;
#21205 = CARTESIAN_POINT ( 'NONE',  ( 0.000000000000000000, 0.000000000000000000, -150.0000000000000000 ) ) ;
#21206 = CARTESIAN_POINT ( 'NONE',  ( -4.204114297095464359, 1.660363174096617156, -3.602136431857887011 ) ) ;
#21207 = EDGE_LOOP ( 'NONE', ( #6040, #16108, #13387, #19765 ) ) ;
#21208 = EDGE_CURVE ( 'NONE', #19693, #11790, #15898, .T. ) ;
#21209 = VERTEX_POINT ( 'NONE', #10113 ) ;
#21210 = LINE ( 'NONE', #17823, #23543 ) ;
#21211 = EDGE_CURVE ( 'NONE', #23797, #2150, #4969, .T. ) ;
#21212 = CARTESIAN_POINT ( 'NONE',  ( 287.4000000000013415, -129.2000000000000455, 146.4928932188134638 ) ) ;
#21214 = CIRCLE ( 'NONE', #261, 145.0000000000000284 ) ;
#21213 = AXIS2_PLACEMENT_3D ( 'NONE', #15157, #9958, #21164 ) ;
#21215 = CIRCLE ( 'NONE', #10834, 0.2000000000000000944 ) ;
#21216 = DIRECTION ( 'NONE',  ( 0.000000000000000000, 0.000000000000000000, 1.000000000000000000 ) ) ;
#21217 = CIRCLE ( 'NONE', #5805, 2.055000000000001492 ) ;
#21218 = EDGE_CURVE ( 'NONE', #6121, #5073, #13870, .T. ) ;
#21219 = PLANE ( 'NONE',  #13475 ) ;
#21220 = PLANE ( 'NONE',  #21562 ) ;
#21221 = CIRCLE ( 'NONE', #10841, 0.2500000000000002220 ) ;
#21222 = DIRECTION ( 'NONE',  ( -0.000000000000000000, 0.4999999999999979461, -0.8660254037844397068 ) ) ;
#21223 = ORIENTED_EDGE ( 'NONE', *, *, #20986, .T. ) ;
#21224 = CARTESIAN_POINT ( 'NONE',  ( 2.500000000000000000, 2.357898499370433054, -1.951563910473907981E-15 ) ) ;
#21225 = DIRECTION ( 'NONE',  ( -0.8090169943749428993, -0.5877852522924793544, 0.000000000000000000 ) ) ;
#21226 = EDGE_CURVE ( 'NONE', #15256, #6626, #14260, .T. ) ;
#21227 = DIRECTION ( 'NONE',  ( 1.000000000000000000, 0.000000000000000000, 0.000000000000000000 ) ) ;
#21228 = ORIENTED_EDGE ( 'NONE', *, *, #1729, .F. ) ;
#21229 = CARTESIAN_POINT ( 'NONE',  ( 4.000000000000000000, 2.309401076758497151, -3.433295621305379353 ) ) ;
#21230 = PRODUCT_CONTEXT ( 'NONE', #3955, 'mechanical' ) ;
#21231 = DIRECTION ( 'NONE',  ( 0.000000000000000000, 0.000000000000000000, -1.000000000000000000 ) ) ;
#21232 = LINE ( 'NONE', #1177, #9414 ) ;
#21233 = AXIS2_PLACEMENT_3D ( 'NONE', #2995, #6644, #17762 ) ;
#21234 = CARTESIAN_POINT ( 'NONE',  ( 52.00000000000000711, -56.79999999999974847, 75.17098115668785852 ) ) ;
#21235 = VECTOR ( 'NONE', #15823, 1000.000000000000000 ) ;
#21236 = DIRECTION ( 'NONE',  ( -0.000000000000000000, -0.000000000000000000, 1.000000000000000000 ) ) ;
#21237 = AXIS2_PLACEMENT_3D ( 'NONE', #12209, #6729, #14010 ) ;
#21238 = VERTEX_POINT ( 'NONE', #12075 ) ;
#21239 = VERTEX_POINT ( 'NONE', #21201 ) ;
#21240 = CARTESIAN_POINT ( 'NONE',  ( -285.2000000000006708, 90.00000000000100897, 34.99999999999999289 ) ) ;
#21241 = CARTESIAN_POINT ( 'NONE',  ( -7.025762299539908296E-16, -8.895730773063899477, -7.917997657324741034 ) ) ;
#21242 = VERTEX_POINT ( 'NONE', #5021 ) ;
#21243 = ORIENTED_EDGE ( 'NONE', *, *, #19459, .T. ) ;
#21244 = CARTESIAN_POINT ( 'NONE',  ( 279.9999999999999432, 273.0299999999999159, 145.0000000000000284 ) ) ;
#21245 = ADVANCED_FACE ( 'NONE', ( #14340 ), #12296, .F. ) ;
#21246 = FACE_OUTER_BOUND ( 'NONE', #11748, .T. ) ;
#21247 = CARTESIAN_POINT ( 'NONE',  ( 2.500000000000002220, 2.357898499370434386, -3.469446951953614189E-15 ) ) ;
#21248 = ORIENTED_EDGE ( 'NONE', *, *, #19013, .F. ) ;
#21249 = EDGE_CURVE ( 'NONE', #21081, #15926, #21568, .T. ) ;
#21250 = LINE ( 'NONE', #12477, #12587 ) ;
#21251 = VERTEX_POINT ( 'NONE', #10219 ) ;
#21252 = CARTESIAN_POINT ( 'NONE',  ( 100.0000000000000000, -1420.000000000000000, 124.9999999999998295 ) ) ;
#21253 = EDGE_CURVE ( 'NONE', #18161, #11805, #6817, .T. ) ;
#21254 = CARTESIAN_POINT ( 'NONE',  ( -7.922281120364393914, -4.573931137438277617, -8.047472243342932430 ) ) ;
#21255 = ORIENTED_EDGE ( 'NONE', *, *, #12059, .F. ) ;
#21256 = ORIENTED_EDGE ( 'NONE', *, *, #8188, .T. ) ;
#21257 = CARTESIAN_POINT ( 'NONE',  ( 132.9250442248338118, 79.72427207779705327, -27.49999999999352340 ) ) ;
#21258 = PRODUCT_DEFINITION_SHAPE ( 'NONE', 'NONE',  #23818 ) ;
#21259 = EDGE_CURVE ( 'NONE', #13380, #7859, #21190, .T. ) ;
#21260 = CARTESIAN_POINT ( 'NONE',  ( 0.5276280594147412240, -4.314175951381924889, -3.320322319201654881 ) ) ;
#21261 = LINE ( 'NONE', #14040, #21525 ) ;
#21262 = DIRECTION ( 'NONE',  ( 0.000000000000000000, 5.551115123125777969E-15, -1.000000000000000000 ) ) ;
#21263 = EDGE_CURVE ( 'NONE', #21906, #13397, #17563, .T. ) ;
#21264 = ORIENTED_EDGE ( 'NONE', *, *, #21277, .T. ) ;
#21265 = DIRECTION ( 'NONE',  ( -1.000000000000000000, 0.000000000000000000, 0.000000000000000000 ) ) ;
#21266 =( REPRESENTATION_RELATIONSHIP ('NONE','NONE', #10127, #21947 ) REPRESENTATION_RELATIONSHIP_WITH_TRANSFORMATION ( #10328 )SHAPE_REPRESENTATION_RELATIONSHIP( ) );
#21267 = ORIENTED_EDGE ( 'NONE', *, *, #21561, .F. ) ;
#21268 = ORIENTED_EDGE ( 'NONE', *, *, #15047, .T. ) ;
#21269 = CARTESIAN_POINT ( 'NONE',  ( 3.266795293236424591, -24.84002319536234538, -145.0000000000000000 ) ) ;
#21270 = ORIENTED_EDGE ( 'NONE', *, *, #1975, .F. ) ;
#21271 = CARTESIAN_POINT ( 'NONE',  ( -65.00000000000000000, -52.79999999999933635, 155.0000000000001421 ) ) ;
#21272 = DIRECTION ( 'NONE',  ( 1.000000000000000000, 0.000000000000000000, 0.000000000000000000 ) ) ;
#21273 = ORIENTED_EDGE ( 'NONE', *, *, #20392, .T. ) ;
#21274 = EDGE_CURVE ( 'NONE', #19104, #22322, #22737, .T. ) ;
#21275 = CARTESIAN_POINT ( 'NONE',  ( -280.2488155364689533, 272.8938770989752811, 146.3689414351990763 ) ) ;
#21276 = CARTESIAN_POINT ( 'NONE',  ( -146.4450000000005332, -494.4690652294800657, -29.99999999999356248 ) ) ;
#21277 = EDGE_CURVE ( 'NONE', #19820, #4309, #12652, .T. ) ;
#21278 = EDGE_LOOP ( 'NONE', ( #17194, #14516, #16294, #2553 ) ) ;
#21279 = ADVANCED_FACE ( 'NONE', ( #9239 ), #20197, .T. ) ;
#21280 = FACE_OUTER_BOUND ( 'NONE', #10022, .T. ) ;
#21281 = EDGE_CURVE ( 'NONE', #16291, #5557, #7052, .T. ) ;
#21282 = CARTESIAN_POINT ( 'NONE',  ( -280.0000000000000568, 269.9999999999999432, 145.0000000000000284 ) ) ;
#21283 = DIRECTION ( 'NONE',  ( -0.7232617928448825673, 0.6905739489807055653, 6.982962677686266711E-15 ) ) ;
#21284 = EDGE_CURVE ( 'NONE', #3693, #11696, #7287, .T. ) ;
#21285 = DIRECTION ( 'NONE',  ( 1.000000000000000000, 0.000000000000000000, 0.000000000000000000 ) ) ;
#21286 = VERTEX_POINT ( 'NONE', #10947 ) ;
#21287 = DIRECTION ( 'NONE',  ( 1.000000000000000000, 0.000000000000000000, 0.000000000000000000 ) ) ;
#21288 = ADVANCED_FACE ( 'NONE', ( #14553 ), #18049, .F. ) ;
#21289 =( NAMED_UNIT ( * ) PLANE_ANGLE_UNIT ( ) SI_UNIT ( $, .RADIAN. ) );
#21291 = VERTEX_POINT ( 'NONE', #16605 ) ;
#21290 = EDGE_LOOP ( 'NONE', ( #11900, #20813, #18263 ) ) ;
#21292 = CARTESIAN_POINT ( 'NONE',  ( -44.99999999999994316, -64.79999999999974136, 250.0000000000003411 ) ) ;
#21293 = CARTESIAN_POINT ( 'NONE',  ( 7.499999999999999112, -1.614186302720606481, -7.450236204328171574 ) ) ;
#21294 = LINE ( 'NONE', #13617, #12801 ) ;
#21295 = DIRECTION ( 'NONE',  ( -0.000000000000000000, -0.000000000000000000, 1.000000000000000000 ) ) ;
#21296 = DIRECTION ( 'NONE',  ( 0.000000000000000000, 0.000000000000000000, 1.000000000000000000 ) ) ;
#21297 = CYLINDRICAL_SURFACE ( 'NONE', #11461, 2.500000000000002220 ) ;
#21298 = ORIENTED_EDGE ( 'NONE', *, *, #5592, .F. ) ;
#21299 = PLANE ( 'NONE',  #2206 ) ;
#21300 = ADVANCED_FACE ( 'NONE', ( #14683 ), #21889, .F. ) ;
#21301 = FACE_BOUND ( 'NONE', #4608, .T. ) ;
#21302 = DIRECTION ( 'NONE',  ( -1.000000000000000000, 3.495664435217746987E-15, 0.000000000000000000 ) ) ;
#21303 = ORIENTED_EDGE ( 'NONE', *, *, #14597, .F. ) ;
#21304 = CARTESIAN_POINT ( 'NONE',  ( 0.1410422978106145031, -4.700232962125109104, -3.687027686973628704 ) ) ;
#21305 = VERTEX_POINT ( 'NONE', #8996 ) ;
#21306 = FACE_OUTER_BOUND ( 'NONE', #10965, .T. ) ;
#21307 = DIRECTION ( 'NONE',  ( 0.6964005597823107463, -0.7176533009294141507, 6.982962677686266711E-15 ) ) ;
#21308 = VERTEX_POINT ( 'NONE', #12538 ) ;
#21309 = CARTESIAN_POINT ( 'NONE',  ( -12.52399064354639613, 21.69904058266284608, -145.0000000000000000 ) ) ;
#21310 = CARTESIAN_POINT ( 'NONE',  ( 0.000000000000000000, 0.000000000000000000, -100.0000000000000000 ) ) ;
#21311 = DIRECTION ( 'NONE',  ( 0.000000000000000000, 0.000000000000000000, 1.000000000000000000 ) ) ;
#21312 = EDGE_CURVE ( 'NONE', #10625, #5401, #3450, .T. ) ;
#21313 = CARTESIAN_POINT ( 'NONE',  ( -90.00000000000000000, -149.9999999999996874, 129.9038105676659711 ) ) ;
#21314 = EDGE_CURVE ( 'NONE', #4934, #9588, #12735, .T. ) ;
#21315 = DIRECTION ( 'NONE',  ( 1.000000000000000000, 0.000000000000000000, -0.000000000000000000 ) ) ;
#21316 = FACE_OUTER_BOUND ( 'NONE', #6991, .T. ) ;
#21317 = VERTEX_POINT ( 'NONE', #14793 ) ;
#21318 = FILL_AREA_STYLE ('',( #10117 ) ) ;
#21319 = CYLINDRICAL_SURFACE ( 'NONE', #16125, 2.649999999999985700 ) ;
#21320 = PLANE ( 'NONE',  #7334 ) ;
#21321 = ORIENTED_EDGE ( 'NONE', *, *, #15908, .F. ) ;
#21322 =( BOUNDED_SURFACE ( )  B_SPLINE_SURFACE ( 3, 2, ( 
 ( #13935, #22926, #6759 ),
 ( #21260, #14156, #953 ),
 ( #1072, #14039, #8459 ),
 ( #4709, #15949, #13807 ),
 ( #23179, #21129, #12012 ),
 ( #19313, #6645, #8332 ) ),
 .UNSPECIFIED., .F., .F., .F. ) 
 B_SPLINE_SURFACE_WITH_KNOTS ( ( 4, 2, 4 ),
 ( 3, 3 ),
 ( 0.02032853247518126918, 0.02278863295364821906, 0.02524873343211517240 ),
 ( 0.000000000000000000, 1.000000000000000000 ),
 .UNSPECIFIED. ) 
 GEOMETRIC_REPRESENTATION_ITEM ( )  RATIONAL_B_SPLINE_SURFACE ( (
 ( 1.000000000000000000, 0.8047781615896837382, 1.000000000000000000),
 ( 1.000000000000000000, 0.8123767586289252218, 1.000000000000000000),
 ( 1.000000000000000000, 0.8190662415564388121, 1.000000000000000000),
 ( 1.000000000000000000, 0.8192361015669026303, 1.000000000000000000),
 ( 1.000000000000000000, 0.8126135807103900266, 1.000000000000000000),
 ( 1.000000000000000000, 0.8047712338318593339, 1.000000000000000000) ) ) 
 REPRESENTATION_ITEM ( '' )  SURFACE ( )  );
#21323 = CIRCLE ( 'NONE', #5508, 2.500000000000002220 ) ;
#21324 = ORIENTED_EDGE ( 'NONE', *, *, #19732, .T. ) ;
#21325 = DIRECTION ( 'NONE',  ( 0.000000000000000000, -0.4999999999999991118, 0.8660254037844390407 ) ) ;
#21326 = DIRECTION ( 'NONE',  ( 0.6568457881071649851, 0.2618274444092050790, 0.7071067811865631159 ) ) ;
#21327 = CARTESIAN_POINT ( 'NONE',  ( 45.24999999999994316, 100.0000000000000000, 147.2000000000005855 ) ) ;
#21328 = CARTESIAN_POINT ( 'NONE',  ( 132.4204480437711879, 80.55959301515328264, 32.37380477188060723 ) ) ;
#21329 = CARTESIAN_POINT ( 'NONE',  ( -285.2000000000000455, 268.1431883566700662, -146.4301685943532618 ) ) ;
#21330 = FACE_BOUND ( 'NONE', #5581, .T. ) ;
#21331 = ORIENTED_EDGE ( 'NONE', *, *, #1321, .F. ) ;
#21332 = DIRECTION ( 'NONE',  ( 1.000000000000000000, 0.000000000000000000, 0.000000000000000000 ) ) ;
#21333 = DIRECTION ( 'NONE',  ( -5.551115123125785858E-15, 5.551115123125785858E-15, -1.000000000000000000 ) ) ;
#21334 = SURFACE_SIDE_STYLE ('',( #1172 ) ) ;
#21335 = EDGE_LOOP ( 'NONE', ( #3703, #2763, #15628, #1656 ) ) ;
#21336 = FILL_AREA_STYLE_COLOUR ( '', #8493 ) ;
#21337 = AXIS2_PLACEMENT_3D ( 'NONE', #4412, #10222, #22875 ) ;
#21338 = CARTESIAN_POINT ( 'NONE',  ( 45.00000000000000000, 272.9999999999999432, 0.000000000000000000 ) ) ;
#21339 = DIRECTION ( 'NONE',  ( 1.110223024625157172E-14, 0.000000000000000000, -1.000000000000000000 ) ) ;
#21340 = CARTESIAN_POINT ( 'NONE',  ( 12.52399064350059277, -1021.699040582693328, -145.0000000000001137 ) ) ;
#21341 = DIRECTION ( 'NONE',  ( 0.000000000000000000, -0.4999999999999992228, 0.8660254037844390407 ) ) ;
#21342 = DIRECTION ( 'NONE',  ( 2.775557561562891351E-17, -1.000000000000000000, 0.000000000000000000 ) ) ;
#21343 = CARTESIAN_POINT ( 'NONE',  ( -285.2000000000000455, 267.7999999999999545, 146.4928932188134354 ) ) ;
#21344 = EDGE_LOOP ( 'NONE', ( #18574, #11832, #21771, #5881 ) ) ;
#21345 = ORIENTED_EDGE ( 'NONE', *, *, #18426, .T. ) ;
#21346 = CARTESIAN_POINT ( 'NONE',  ( -280.6839617489741840, 269.4578961534455175, -146.4533442688710920 ) ) ;
#21347 = CARTESIAN_POINT ( 'NONE',  ( -67.34999999999996589, -87.33333333333338544, 145.0000000000000000 ) ) ;
#21348 = ORIENTED_EDGE ( 'NONE', *, *, #7617, .F. ) ;
#21349 = VECTOR ( 'NONE', #2384, 1000.000000000000000 ) ;
#21350 = B_SPLINE_SURFACE_WITH_KNOTS ( 'NONE', 1, 3, ( 
 ( #13193, #10764, #5652, #23649, #18109, #1415, #1670, #16415, #9051, #14494 ),
 ( #7458, #22181, #16762, #7578, #14969, #7110, #1564, #8948, #16305, #11473 ),
 ( #17126, #9525, #22897, #22540, #17019, #6259, #472, #13778, #15326, #20870 ),
 ( #4323, #19156, #22427, #5888, #11612, #7825, #2619, #15209, #13665, #22795 ) ),
 .UNSPECIFIED., .F., .F., .F.,
 ( 2, 1, 1, 2 ),
 ( 4, 2, 2, 2, 4 ),
 ( -0.01000000000000000021, 0.000000000000000000, 1.000000000000000000, 1.010099999999999998 ),
 ( 0.000000000000000000, 0.2500000000000000000, 0.5000000000000000000, 0.7500000000000000000, 1.000000000000000000 ),
 .UNSPECIFIED. ) ;
#21351 = CARTESIAN_POINT ( 'NONE',  ( 25.00000000000001066, 45.00100000000043821, 64.99999999999984368 ) ) ;
#21352 = AXIS2_PLACEMENT_3D ( 'NONE', #19726, #10584, #17923 ) ;
#21353 = EDGE_LOOP ( 'NONE', ( #5181, #5569, #6546, #19247 ) ) ;
#21354 = LINE ( 'NONE', #2983, #23293 ) ;
#21355 = CARTESIAN_POINT ( 'NONE',  ( -126.7581711459448712, 89.20411804604300698, 28.46749050845386009 ) ) ;
#21356 = ORIENTED_EDGE ( 'NONE', *, *, #4889, .F. ) ;
#21357 = CARTESIAN_POINT ( 'NONE',  ( 5.384454397937118664, 0.000000000000000000, -4.484454397937119197 ) ) ;
#21358 = ORIENTED_EDGE ( 'NONE', *, *, #21985, .T. ) ;
#21359 = FACE_OUTER_BOUND ( 'NONE', #8976, .T. ) ;
#21360 = FACE_OUTER_BOUND ( 'NONE', #22923, .T. ) ;
#21361 = ORIENTED_EDGE ( 'NONE', *, *, #10326, .T. ) ;
#21362 = ORIENTED_EDGE ( 'NONE', *, *, #1145, .F. ) ;
#21363 = CARTESIAN_POINT ( 'NONE',  ( 235.0000000000000284, -489.9999999999998863, 57.00000000000002132 ) ) ;
#21364 = DIRECTION ( 'NONE',  ( 0.8823264512277401161, 0.4706379005816069272, 1.080538264299094565E-16 ) ) ;
#21365 = CARTESIAN_POINT ( 'NONE',  ( -281.1807969192698238, 269.4810649015077502, -149.9324007871373112 ) ) ;
#21366 = AXIS2_PLACEMENT_3D ( 'NONE', #12814, #3561, #20115 ) ;
#21367 = FACE_BOUND ( 'NONE', #5598, .T. ) ;
#21368 = DIRECTION ( 'NONE',  ( -1.000000000000000000, -0.000000000000000000, -0.000000000000000000 ) ) ;
#21369 = ADVANCED_FACE ( 'NONE', ( #13006 ), #22124, .T. ) ;
#21370 = VERTEX_POINT ( 'NONE', #23706 ) ;
#21371 = LINE ( 'NONE', #4713, #10302 ) ;
#21372 = ADVANCED_FACE ( 'NONE', ( #18168 ), #19621, .F. ) ;
#21373 = ADVANCED_FACE ( 'NONE', ( #7163 ), #10840, .F. ) ;
#21374 = ORIENTED_EDGE ( 'NONE', *, *, #5116, .T. ) ;
#21375 = EDGE_CURVE ( 'NONE', #11798, #10799, #11061, .T. ) ;
#21376 = VERTEX_POINT ( 'NONE', #3768 ) ;
#21377 = VECTOR ( 'NONE', #15651, 1000.000000000000000 ) ;
#21378 = DIRECTION ( 'NONE',  ( -0.000000000000000000, -0.000000000000000000, 1.000000000000000000 ) ) ;
#21379 = VECTOR ( 'NONE', #8174, 1000.000000000000114 ) ;
#21380 = EDGE_LOOP ( 'NONE', ( #15381, #6022 ) ) ;
#21381 = CARTESIAN_POINT ( 'NONE',  ( 7.968863443239234456, 4.547634245050474533, -8.057411785091787237 ) ) ;
#21382 = CARTESIAN_POINT ( 'NONE',  ( 2.999999999999999112, 20.30000000000000071, 0.000000000000000000 ) ) ;
#21383 = AXIS2_PLACEMENT_3D ( 'NONE', #16866, #2005, #9393 ) ;
#21384 = ORIENTED_EDGE ( 'NONE', *, *, #16181, .F. ) ;
#21385 = DIRECTION ( 'NONE',  ( -0.000000000000000000, -0.000000000000000000, 1.000000000000000000 ) ) ;
#21386 = DIRECTION ( 'NONE',  ( -0.000000000000000000, -0.000000000000000000, 1.000000000000000000 ) ) ;
#21387 = VERTEX_POINT ( 'NONE', #1968 ) ;
#21388 = DIRECTION ( 'NONE',  ( 0.000000000000000000, -3.491481338843133355E-15, -1.000000000000000000 ) ) ;
#21389 = CARTESIAN_POINT ( 'NONE',  ( 7.922281120364393914, -4.573931137438282057, -8.047472243342932430 ) ) ;
#21390 = CARTESIAN_POINT ( 'NONE',  ( 40.00000000000000000, 100.0000000000000000, 147.2000000000005855 ) ) ;
#21391 = APPLICATION_CONTEXT ( 'automotive_design' ) ;
#21392 = CARTESIAN_POINT ( 'NONE',  ( 0.000000000000000000, 0.000000000000000000, -90.00000000000000000 ) ) ;
#21393 = ORIENTED_EDGE ( 'NONE', *, *, #16315, .T. ) ;
#21394 = EDGE_CURVE ( 'NONE', #1127, #14717, #13883, .T. ) ;
#21396 = EDGE_LOOP ( 'NONE', ( #7962, #12667, #16547, #22704 ) ) ;
#21395 = VERTEX_POINT ( 'NONE', #19302 ) ;
#21397 = DIRECTION ( 'NONE',  ( 0.000000000000000000, 0.000000000000000000, 1.000000000000000000 ) ) ;
#21398 = DIRECTION ( 'NONE',  ( -0.000000000000000000, 1.000000000000000000, 0.000000000000000000 ) ) ;
#21399 = CARTESIAN_POINT ( 'NONE',  ( -90.00000000000000000, 75.00000000000001421, 0.000000000000000000 ) ) ;
#21400 = ADVANCED_FACE ( 'NONE', ( #5480 ), #1093, .F. ) ;
#21401 = CARTESIAN_POINT ( 'NONE',  ( -280.0000000000000568, 272.9999999999999432, -144.9999999999999716 ) ) ;
#21402 = EDGE_CURVE ( 'NONE', #8982, #5006, #17561, .T. ) ;
#21403 = CYLINDRICAL_SURFACE ( 'NONE', #10427, 2.649999999999971934 ) ;
#21404 = FACE_OUTER_BOUND ( 'NONE', #438, .T. ) ;
#21405 = AXIS2_PLACEMENT_3D ( 'NONE', #4451, #22673, #4334 ) ;
#21406 = VERTEX_POINT ( 'NONE', #16824 ) ;
#21407 = PLANE ( 'NONE',  #8793 ) ;
#21408 = EDGE_CURVE ( 'NONE', #15333, #17002, #3037, .T. ) ;
#21409 = VERTEX_POINT ( 'NONE', #2082 ) ;
#21410 = EDGE_CURVE ( 'NONE', #9726, #20363, #23497, .T. ) ;
#21411 = CARTESIAN_POINT ( 'NONE',  ( 0.000000000000000000, 1.178949249685213863, -2.042000000000001148 ) ) ;
#21412 = DIRECTION ( 'NONE',  ( 1.000000000000000000, 0.000000000000000000, 0.000000000000000000 ) ) ;
#21413 = ITEM_DEFINED_TRANSFORMATION ( 'NONE', 'NONE', #3464,  #11210 ) ;
#21414 = VERTEX_POINT ( 'NONE', #12145 ) ;
#21415 = VECTOR ( 'NONE', #8452, 1000.000000000000000 ) ;
#21416 = LINE ( 'NONE', #17671, #19845 ) ;
#21417 = VERTEX_POINT ( 'NONE', #17895 ) ;
#21418 = DIRECTION ( 'NONE',  ( -1.000000000000000000, -2.775557561562891351E-17, 0.000000000000000000 ) ) ;
#21419 = ORIENTED_EDGE ( 'NONE', *, *, #3574, .F. ) ;
#21420 = CARTESIAN_POINT ( 'NONE',  ( -281.1810844504668125, 269.4795879751483767, 149.9329465209280272 ) ) ;
#21421 = CYLINDRICAL_SURFACE ( 'NONE', #15788, 7.500000000000007105 ) ;
#21422 = CARTESIAN_POINT ( 'NONE',  ( -90.00000000000000000, -76.73205080756885366, 3.000000000000002665 ) ) ;
#21423 = DIRECTION ( 'NONE',  ( -0.7071067811865310304, 0.000000000000000000, 0.7071067811865641151 ) ) ;
#21424 = CARTESIAN_POINT ( 'NONE',  ( -282.2000000000000455, 267.7999999999999545, -146.4928932188134354 ) ) ;
#21425 = CIRCLE ( 'NONE', #3301, 5.249999999999949374 ) ;
#21426 = DIRECTION ( 'NONE',  ( -1.000000000000000000, 3.495664435217746987E-15, 0.000000000000000000 ) ) ;
#21427 = DIRECTION ( 'NONE',  ( -1.000000000000000000, -0.000000000000000000, -0.000000000000000000 ) ) ;
#21428 = EDGE_LOOP ( 'NONE', ( #18632, #12373, #3961, #18230, #12350 ) ) ;
#21429 = AXIS2_PLACEMENT_3D ( 'NONE', #21143, #2888, #23426 ) ;
#21430 = CARTESIAN_POINT ( 'NONE',  ( 0.000000000000000000, 0.000000000000000000, -4.974599999999998801 ) ) ;
#21431 = CARTESIAN_POINT ( 'NONE',  ( -4.000000000000000000, -0.8232339106130515116, -3.430630286862743183 ) ) ;
#21432 = VERTEX_POINT ( 'NONE', #8249 ) ;
#21433 = VECTOR ( 'NONE', #23106, 1000.000000000000000 ) ;
#21434 = ORIENTED_EDGE ( 'NONE', *, *, #2270, .T. ) ;
#21435 = CARTESIAN_POINT ( 'NONE',  ( 5.000000000000000000, -4.685197434473811207, 4.770489558936219510E-15 ) ) ;
#21436 = DIRECTION ( 'NONE',  ( -0.8191520442889907994, 0.000000000000000000, -0.5735764363510474917 ) ) ;
#21437 =( REPRESENTATION_RELATIONSHIP ('NONE','NONE', #10127, #5587 ) REPRESENTATION_RELATIONSHIP_WITH_TRANSFORMATION ( #12878 )SHAPE_REPRESENTATION_RELATIONSHIP( ) );
#21439 = CARTESIAN_POINT ( 'NONE',  ( 67.35000000000002274, -112.6666666666666714, 0.000000000000000000 ) ) ;
#21438 = PRODUCT_DEFINITION_SHAPE ( 'NONE', 'NONE',  #23835 ) ;
#21440 = EDGE_CURVE ( 'NONE', #1247, #9060, #19568, .T. ) ;
#21441 = ADVANCED_FACE ( 'NONE', ( #19446 ), #17649, .F. ) ;
#21442 = VECTOR ( 'NONE', #10818, 1000.000000000000000 ) ;
#21443 = CARTESIAN_POINT ( 'NONE',  ( 4.024499207728657879, -2.323545700935587988, -3.572172305156509964 ) ) ;
#21444 = ADVANCED_FACE ( 'NONE', ( #8605 ), #23323, .F. ) ;
#21445 = DIRECTION ( 'NONE',  ( 6.982962677686266711E-15, -9.837870180509810443E-29, 1.000000000000000000 ) ) ;
#21446 = ORIENTED_EDGE ( 'NONE', *, *, #7831, .F. ) ;
#21447 = CARTESIAN_POINT ( 'NONE',  ( 132.8404720734533555, 79.86494211668889420, -27.49999999999351985 ) ) ;
#21448 = ORIENTED_EDGE ( 'NONE', *, *, #15339, .F. ) ;
#21449 = CYLINDRICAL_SURFACE ( 'NONE', #20261, 145.0000000000000284 ) ;
#21450 = DIRECTION ( 'NONE',  ( 0.000000000000000000, 0.000000000000000000, -1.000000000000000000 ) ) ;
#21451 = DIRECTION ( 'NONE',  ( 0.000000000000000000, 0.000000000000000000, 1.000000000000000000 ) ) ;
#21452 = EDGE_LOOP ( 'NONE', ( #5843, #18132, #1931, #15519 ) ) ;
#21453 = CARTESIAN_POINT ( 'NONE',  ( 4.000000000000000888, 1.539600717838996990, -3.300726591567079815 ) ) ;
#21454 = DIRECTION ( 'NONE',  ( -0.000000000000000000, 0.000000000000000000, -1.000000000000000000 ) ) ;
#21455 = DIRECTION ( 'NONE',  ( -1.000000000000000000, -0.000000000000000000, -0.000000000000000000 ) ) ;
#21456 = PLANE ( 'NONE',  #14816 ) ;
#21457 = DIRECTION ( 'NONE',  ( -1.000000000000000000, 0.000000000000000000, 0.000000000000000000 ) ) ;
#21458 = FACE_OUTER_BOUND ( 'NONE', #21207, .T. ) ;
#21459 = CARTESIAN_POINT ( 'NONE',  ( -1.994931997373328159E-14, -8.660254037844390851, -1.000000000000000888 ) ) ;
#21460 = ORIENTED_EDGE ( 'NONE', *, *, #22440, .F. ) ;
#21461 = ORIENTED_EDGE ( 'NONE', *, *, #18076, .F. ) ;
#21462 = CARTESIAN_POINT ( 'NONE',  ( -85.22886158240879695, 117.3074641843673049, 90.00000000000000000 ) ) ;
#21463 = CIRCLE ( 'NONE', #7966, 2.500000000000002220 ) ;
#21464 = DIRECTION ( 'NONE',  ( 0.000000000000000000, 0.000000000000000000, 1.000000000000000000 ) ) ;
#21465 = EDGE_LOOP ( 'NONE', ( #14775, #14417, #3587, #15667 ) ) ;
#21466 = VERTEX_POINT ( 'NONE', #10306 ) ;
#21467 = LINE ( 'NONE', #4929, #20439 ) ;
#21468 = CARTESIAN_POINT ( 'NONE',  ( 2.804994570502171047, 3.229033611042449792, -3.526374918436834704 ) ) ;
#21469 = B_SPLINE_CURVE_WITH_KNOTS ( 'NONE', 3,
 ( #12941, #5530, #5421, #16408, #23756, #14602 ),
 .UNSPECIFIED., .F., .F.,
 ( 4, 2, 4 ),
 ( 0.000000000000000000, 0.0004189869898914161677, 0.0008379739797828302753 ),
 .UNSPECIFIED. ) ;
#21470 = ORIENTED_EDGE ( 'NONE', *, *, #17834, .F. ) ;
#21471 = CARTESIAN_POINT ( 'NONE',  ( 280.6220388411721274, 271.9822575857424454, 148.2140793454688037 ) ) ;
#21472 = DIRECTION ( 'NONE',  ( 1.000000000000000000, 0.000000000000000000, 0.000000000000000000 ) ) ;
#21473 = ORIENTED_EDGE ( 'NONE', *, *, #22276, .F. ) ;
#21474 = EDGE_CURVE ( 'NONE', #17002, #15333, #9238, .T. ) ;
#21475 = DIRECTION ( 'NONE',  ( 0.000000000000000000, 1.000000000000000000, -1.103561164596346103E-15 ) ) ;
#21476 = AXIS2_PLACEMENT_3D ( 'NONE', #19683, #1323, #23052 ) ;
#21477 = EDGE_LOOP ( 'NONE', ( #1214, #1854, #7194, #20931 ) ) ;
#21478 = EDGE_CURVE ( 'NONE', #11453, #20774, #15979, .T. ) ;
#21479 = CIRCLE ( 'NONE', #7214, 19.99999999999999645 ) ;
#21480 = DIRECTION ( 'NONE',  ( 0.000000000000000000, -3.495664435217746987E-15, 1.000000000000000000 ) ) ;
#21481 = FACE_BOUND ( 'NONE', #11981, .T. ) ;
#21482 = ORIENTED_EDGE ( 'NONE', *, *, #14838, .T. ) ;
#21483 = VERTEX_POINT ( 'NONE', #22843 ) ;
#21484 = CARTESIAN_POINT ( 'NONE',  ( 133.8109447024532983, 78.22816056888444791, -28.34359615383082343 ) ) ;
#21485 = DIRECTION ( 'NONE',  ( 1.000000000000000000, 0.000000000000000000, 0.000000000000000000 ) ) ;
#21486 = CARTESIAN_POINT ( 'NONE',  ( -280.9953931959807392, 270.4054396500289954, -149.5132312761074047 ) ) ;
#21487 = CARTESIAN_POINT ( 'NONE',  ( -4.599534470795546781, 6.460478697738500031, -7.590212325761530821 ) ) ;
#21488 = DIRECTION ( 'NONE',  ( -1.000000000000000000, -0.000000000000000000, -0.000000000000000000 ) ) ;
#21489 = ORIENTED_EDGE ( 'NONE', *, *, #7973, .F. ) ;
#21490 = DIRECTION ( 'NONE',  ( 1.000000000000000000, 0.000000000000000000, 0.000000000000000000 ) ) ;
#21491 = ORIENTED_EDGE ( 'NONE', *, *, #5924, .T. ) ;
#21492 = AXIS2_PLACEMENT_3D ( 'NONE', #20295, #5580, #3753 ) ;
#21493 = VECTOR ( 'NONE', #23149, 1000.000000000000000 ) ;
#21494 = EDGE_CURVE ( 'NONE', #18839, #12455, #6309, .T. ) ;
#21495 = EDGE_LOOP ( 'NONE', ( #137, #11157, #8810, #12868 ) ) ;
#21496 = CARTESIAN_POINT ( 'NONE',  ( -280.0000000000000568, 272.9999999999999432, -144.9999999999999716 ) ) ;
#21497 = ORIENTED_EDGE ( 'NONE', *, *, #20664, .F. ) ;
#21498 = DIRECTION ( 'NONE',  ( 0.000000000000000000, 0.000000000000000000, 1.000000000000000000 ) ) ;
#21499 = ORIENTED_EDGE ( 'NONE', *, *, #2241, .F. ) ;
#21500 = EDGE_CURVE ( 'NONE', #17208, #15945, #8494, .T. ) ;
#21501 = CARTESIAN_POINT ( 'NONE',  ( -135.9487776228373264, -1074.451030117130358, 32.48389983298811501 ) ) ;
#21502 = CARTESIAN_POINT ( 'NONE',  ( -146.0000000000005400, -494.4690652294800657, -32.05499999999356930 ) ) ;
#21503 = EDGE_CURVE ( 'NONE', #8260, #846, #17701, .T. ) ;
#21504 = EDGE_LOOP ( 'NONE', ( #7224, #13604, #12029, #4582 ) ) ;
#21505 = FACE_OUTER_BOUND ( 'NONE', #13442, .T. ) ;
#21506 = CARTESIAN_POINT ( 'NONE',  ( 235.0000000000000284, -490.0000000000001137, -56.99999999999996447 ) ) ;
#21507 = EDGE_CURVE ( 'NONE', #829, #15265, #2905, .T. ) ;
#21508 = VECTOR ( 'NONE', #16005, 1000.000000000000000 ) ;
#21509 = CARTESIAN_POINT ( 'NONE',  ( 0.000000000000000000, 0.000000000000000000, -90.00000000000000000 ) ) ;
#21510 = CARTESIAN_POINT ( 'NONE',  ( 124.8578076529639702, -1091.845273256946484, -27.57873596473014643 ) ) ;
#21511 = AXIS2_PLACEMENT_3D ( 'NONE', #17165, #21708, #2423 ) ;
#21512 = CARTESIAN_POINT ( 'NONE',  ( 57.99999999999997868, -62.00000000000001421, 5.199999999999997513 ) ) ;
#21513 = VERTEX_POINT ( 'NONE', #19338 ) ;
#21514 =( NAMED_UNIT ( * ) PLANE_ANGLE_UNIT ( ) SI_UNIT ( $, .RADIAN. ) );
#21516 = VERTEX_POINT ( 'NONE', #22957 ) ;
#21515 = VERTEX_POINT ( 'NONE', #2797 ) ;
#21517 = DIRECTION ( 'NONE',  ( 6.123233995736766036E-17, 0.000000000000000000, -1.000000000000000000 ) ) ;
#21518 = DIRECTION ( 'NONE',  ( 1.000000000000000000, 0.000000000000000000, 0.000000000000000000 ) ) ;
#21519 = DIRECTION ( 'NONE',  ( -0.9423651898111408132, -0.3345860861306287348, 6.982962677686266711E-15 ) ) ;
#21520 = DIRECTION ( 'NONE',  ( -8.144298233840332611E-17, 0.000000000000000000, -1.000000000000000000 ) ) ;
#21521 = DIRECTION ( 'NONE',  ( 0.000000000000000000, 0.000000000000000000, -1.000000000000000000 ) ) ;
#21522 = AXIS2_PLACEMENT_3D ( 'NONE', #12746, #8846, #20058 ) ;
#21523 = CIRCLE ( 'NONE', #22676, 2.041999999999999815 ) ;
#21524 = ORIENTED_EDGE ( 'NONE', *, *, #7703, .T. ) ;
#21525 = VECTOR ( 'NONE', #4710, 1000.000000000000000 ) ;
#21526 = CARTESIAN_POINT ( 'NONE',  ( 7.500000000000001776, 0.000000000000000000, 0.000000000000000000 ) ) ;
#21527 = CIRCLE ( 'NONE', #9580, 4.250000000000000000 ) ;
#21528 = VERTEX_POINT ( 'NONE', #6788 ) ;
#21529 = EDGE_CURVE ( 'NONE', #3010, #22378, #6426, .T. ) ;
#21530 = ADVANCED_FACE ( 'NONE', ( #13838 ), #14629, .T. ) ;
#21531 = DIRECTION ( 'NONE',  ( -0.000000000000000000, -0.000000000000000000, 1.000000000000000000 ) ) ;
#21532 = FACE_OUTER_BOUND ( 'NONE', #19598, .T. ) ;
#21533 = CONTEXT_DEPENDENT_SHAPE_REPRESENTATION ( #18509, #13583 ) ;
#21534 = ORIENTED_EDGE ( 'NONE', *, *, #6055, .T. ) ;
#21535 = CARTESIAN_POINT ( 'NONE',  ( -121.5574576620399654, 79.04925354955206274, -90.00000000000000000 ) ) ;
#21536 = EDGE_LOOP ( 'NONE', ( #4739, #15961 ) ) ;
#21537 = CARTESIAN_POINT ( 'NONE',  ( -129.2813770747751789, 85.50638651249015254, -30.65604281379820861 ) ) ;
#21538 = DIRECTION ( 'NONE',  ( -0.000000000000000000, 1.000000000000000000, 0.000000000000000000 ) ) ;
#21539 = ORIENTED_EDGE ( 'NONE', *, *, #18331, .F. ) ;
#21540 = DIRECTION ( 'NONE',  ( 3.700743415417189520E-15, 1.000000000000000000, 0.000000000000000000 ) ) ;
#21541 = EDGE_CURVE ( 'NONE', #286, #9681, #1349, .T. ) ;
#21542 = DIRECTION ( 'NONE',  ( -1.000000000000000000, -2.775557561562891351E-17, 0.000000000000000000 ) ) ;
#21543 = PLANE ( 'NONE',  #19973 ) ;
#21544 = ADVANCED_FACE ( 'NONE', ( #4625 ), #16190, .T. ) ;
#21545 = PRODUCT_DEFINITION_SHAPE ( 'NONE', 'NONE',  #19197 ) ;
#21546 = AXIS2_PLACEMENT_3D ( 'NONE', #13556, #15570, #11355 ) ;
#21547 = DIRECTION ( 'NONE',  ( 0.000000000000000000, 0.000000000000000000, 1.000000000000000000 ) ) ;
#21548 = CIRCLE ( 'NONE', #5740, 2.055000000000001492 ) ;
#21549 = LINE ( 'NONE', #8527, #721 ) ;
#21551 = AXIS2_PLACEMENT_3D ( 'NONE', #12640, #17802, #6928 ) ;
#21550 = DIRECTION ( 'NONE',  ( 0.000000000000000000, -2.618450529776326854E-15, -1.000000000000000000 ) ) ;
#21552 = VECTOR ( 'NONE', #7554, 1000.000000000000114 ) ;
#21553 = CARTESIAN_POINT ( 'NONE',  ( 145.9999999999998010, -801.0618695410399823, 30.00000000000641620 ) ) ;
#21554 = CIRCLE ( 'NONE', #1478, 2.499999999999998668 ) ;
#21555 = EDGE_CURVE ( 'NONE', #11696, #17056, #23086, .T. ) ;
#21556 = ORIENTED_EDGE ( 'NONE', *, *, #13297, .T. ) ;
#21557 = PRODUCT_DEFINITION ( 'UNKNOWN', '', #9275, #16773 ) ;
#21558 =( NAMED_UNIT ( * ) SI_UNIT ( $, .STERADIAN. ) SOLID_ANGLE_UNIT ( ) );
#21559 = DIRECTION ( 'NONE',  ( 0.000000000000000000, 0.000000000000000000, 1.000000000000000000 ) ) ;
#21560 = CYLINDRICAL_SURFACE ( 'NONE', #15842, 145.0000000000000284 ) ;
#21561 = EDGE_CURVE ( 'NONE', #17916, #12643, #5764, .T. ) ;
#21562 = AXIS2_PLACEMENT_3D ( 'NONE', #3193, #4676, #14232 ) ;
#21563 = EDGE_LOOP ( 'NONE', ( #17984, #21177 ) ) ;
#21564 = EDGE_LOOP ( 'NONE', ( #5293, #21491, #11671, #20970 ) ) ;
#21565 = DIRECTION ( 'NONE',  ( 1.000000000000000000, -1.408839003528726857E-14, -6.982962677686266711E-15 ) ) ;
#21566 = CARTESIAN_POINT ( 'NONE',  ( 45.00000000000002132, -59.79999999999933635, 195.0000000000002558 ) ) ;
#21567 = LINE ( 'NONE', #5035, #12579 ) ;
#21568 = CIRCLE ( 'NONE', #8086, 0.3000000000000016542 ) ;
#21569 = CARTESIAN_POINT ( 'NONE',  ( 0.000000000000000000, 0.000000000000000000, -90.00000000000000000 ) ) ;
#21570 = TOROIDAL_SURFACE ( 'NONE', #1515, 22.50000000000000000, 1.500000000000000444 ) ;
#21571 = DIRECTION ( 'NONE',  ( -1.000000000000000000, 1.408839003528726857E-14, 6.982962677686266711E-15 ) ) ;
#21572 = VECTOR ( 'NONE', #11451, 1000.000000000000000 ) ;
#21573 = ORIENTED_EDGE ( 'NONE', *, *, #9786, .F. ) ;
#21574 = AXIS2_PLACEMENT_3D ( 'NONE', #7152, #1710, #3526 ) ;
#21575 = AXIS2_PLACEMENT_3D ( 'NONE', #11841, #6608, #15565 ) ;
#21576 = FACE_OUTER_BOUND ( 'NONE', #17395, .T. ) ;
#21577 = VERTEX_POINT ( 'NONE', #4858 ) ;
#21578 = LINE ( 'NONE', #6610, #16031 ) ;
#21579 = CARTESIAN_POINT ( 'NONE',  ( 0.000000000000000000, 269.9999999999999432, 0.000000000000000000 ) ) ;
#21580 = EDGE_CURVE ( 'NONE', #9425, #20571, #12265, .T. ) ;
#21581 = FILL_AREA_STYLE ('',( #4913 ) ) ;
#21582 = VERTEX_POINT ( 'NONE', #16225 ) ;
#21583 = FACE_OUTER_BOUND ( 'NONE', #16841, .T. ) ;
#21584 =( REPRESENTATION_RELATIONSHIP ('NONE','NONE', #10127, #4815 ) REPRESENTATION_RELATIONSHIP_WITH_TRANSFORMATION ( #17250 )SHAPE_REPRESENTATION_RELATIONSHIP( ) );
#21585 = CARTESIAN_POINT ( 'NONE',  ( 5.047120108843200725, -5.746297884371399434, -0.1007566405101860824 ) ) ;
#21586 = DIRECTION ( 'NONE',  ( 0.000000000000000000, 0.000000000000000000, 1.000000000000000000 ) ) ;
#21587 = DIRECTION ( 'NONE',  ( -1.000000000000000000, -0.000000000000000000, -0.000000000000000000 ) ) ;
#21588 = EDGE_CURVE ( 'NONE', #11181, #22508, #21754, .T. ) ;
#21589 = DIRECTION ( 'NONE',  ( -1.000000000000000000, 3.495664435217746987E-15, 0.000000000000000000 ) ) ;
#21590 = CARTESIAN_POINT ( 'NONE',  ( -31.74999999999995737, 0.000000000000000000, 0.000000000000000000 ) ) ;
#21591 = CARTESIAN_POINT ( 'NONE',  ( -72.64999999999994884, -112.6666666666667140, 3.000000000000001332 ) ) ;
#21592 = ORIENTED_EDGE ( 'NONE', *, *, #19363, .F. ) ;
#21593 = EDGE_CURVE ( 'NONE', #2320, #23165, #1513, .T. ) ;
#21595 = EDGE_LOOP ( 'NONE', ( #23248, #3226 ) ) ;
#21594 = EDGE_CURVE ( 'NONE', #11975, #16945, #8969, .T. ) ;
#21597 = AXIS2_PLACEMENT_3D ( 'NONE', #21063, #17673, #2819 ) ;
#21596 = AXIS2_PLACEMENT_3D ( 'NONE', #10092, #2333, #18870 ) ;
#21598 = CARTESIAN_POINT ( 'NONE',  ( 279.9999999999999432, 269.9999999999999432, 145.0000000000000284 ) ) ;
#21599 = EDGE_CURVE ( 'NONE', #1127, #874, #11569, .T. ) ;
#21600 = AXIS2_PLACEMENT_3D ( 'NONE', #18248, #21518, #8861 ) ;
#21601 = ORIENTED_EDGE ( 'NONE', *, *, #21115, .T. ) ;
#21602 = AXIS2_PLACEMENT_3D ( 'NONE', #18235, #11274, #9324 ) ;
#21603 = AXIS2_PLACEMENT_3D ( 'NONE', #1523, #23375, #10725 ) ;
#21604 = PLANE ( 'NONE',  #7667 ) ;
#21605 = DIRECTION ( 'NONE',  ( -0.000000000000000000, 1.000000000000000000, -3.469446951953613794E-15 ) ) ;
#21606 = ORIENTED_EDGE ( 'NONE', *, *, #16312, .T. ) ;
#21607 = CARTESIAN_POINT ( 'NONE',  ( 280.4976310729377360, 269.6958543268121957, 146.0927021017107563 ) ) ;
#21608 = CARTESIAN_POINT ( 'NONE',  ( -45.00000000000000000, 272.9999999999999432, -5.249999999999973355 ) ) ;
#21609 = EDGE_LOOP ( 'NONE', ( #13797, #4121, #13050, #22302 ) ) ;
#21610 = CARTESIAN_POINT ( 'NONE',  ( -134.6139742523217251, -1076.838024977515715, -29.18615827854494782 ) ) ;
#21611 = EDGE_LOOP ( 'NONE', ( #13688, #21152, #15156, #21017, #23007, #7561, #8344, #11775, #16525, #4572 ) ) ;
#21612 = AXIS2_PLACEMENT_3D ( 'NONE', #16690, #3746, #11289 ) ;
#21613 = DIRECTION ( 'NONE',  ( 1.000000000000000000, 0.000000000000000000, 0.000000000000000000 ) ) ;
#21614 = STYLED_ITEM ( 'NONE', ( #4957 ), #5011 ) ;
#21616 = AXIS2_PLACEMENT_3D ( 'NONE', #18548, #18308, #1547 ) ;
#21615 = CARTESIAN_POINT ( 'NONE',  ( -40.00000000000000000, 100.0000000000000000, 150.2000000000009550 ) ) ;
#21617 = ORIENTED_EDGE ( 'NONE', *, *, #14844, .F. ) ;
#21618 = VERTEX_POINT ( 'NONE', #36 ) ;
#21619 = CARTESIAN_POINT ( 'NONE',  ( 132.9260832389180962, 79.72254387117985175, -32.49999999999352696 ) ) ;
#21620 = AXIS2_PLACEMENT_3D ( 'NONE', #6516, #12365, #3136 ) ;
#21621 = AXIS2_PLACEMENT_3D ( 'NONE', #19138, #6596, #803 ) ;
#21622 = DIRECTION ( 'NONE',  ( -1.000000000000000000, 0.000000000000000000, 6.123233995736766036E-17 ) ) ;
#21623 = DIRECTION ( 'NONE',  ( 0.000000000000000000, -1.000000000000000000, 0.000000000000000000 ) ) ;
#21624 = CARTESIAN_POINT ( 'NONE',  ( -282.2000000000007276, 75.00000000000098055, 90.00000000000000000 ) ) ;
#21625 = CARTESIAN_POINT ( 'NONE',  ( 0.000000000000000000, 0.000000000000000000, 0.000000000000000000 ) ) ;
#21626 = ORIENTED_EDGE ( 'NONE', *, *, #3733, .T. ) ;
#21627 = EDGE_CURVE ( 'NONE', #10418, #3759, #7285, .T. ) ;
#21628 = CARTESIAN_POINT ( 'NONE',  ( -285.2000000000006708, 90.00000000000100897, 34.99999999999999289 ) ) ;
#21629 = EDGE_CURVE ( 'NONE', #17037, #7464, #1811, .T. ) ;
#21630 = ORIENTED_EDGE ( 'NONE', *, *, #23317, .T. ) ;
#21631 = EDGE_CURVE ( 'NONE', #14223, #17523, #7383, .T. ) ;
#21632 = VECTOR ( 'NONE', #209, 1000.000000000000000 ) ;
#21633 = ORIENTED_EDGE ( 'NONE', *, *, #2547, .T. ) ;
#21634 = DIRECTION ( 'NONE',  ( 0.000000000000000000, 0.000000000000000000, -1.000000000000000000 ) ) ;
#21635 = VERTEX_POINT ( 'NONE', #12976 ) ;
#21636 = CARTESIAN_POINT ( 'NONE',  ( 2.387978478801324300, 7.281554020289410012, -7.069802615102035226 ) ) ;
#21637 = EDGE_LOOP ( 'NONE', ( #20287, #12286, #2713, #2625 ) ) ;
#21638 = VERTEX_POINT ( 'NONE', #3270 ) ;
#21639 = CARTESIAN_POINT ( 'NONE',  ( -90.00000000000000000, -152.9999999999996874, 129.9038105676659711 ) ) ;
#21640 = CARTESIAN_POINT ( 'NONE',  ( -45.00000000000000711, 0.000000000000000000, 20.00000000000000000 ) ) ;
#21641 = FACE_OUTER_BOUND ( 'NONE', #23097, .T. ) ;
#21642 = DIRECTION ( 'NONE',  ( 1.000000000000000000, 0.000000000000000000, 0.000000000000000000 ) ) ;
#21643 = CARTESIAN_POINT ( 'NONE',  ( -1.500000000000000000, 12.00000000000000000, 0.000000000000000000 ) ) ;
#21644 = ORIENTED_EDGE ( 'NONE', *, *, #13969, .F. ) ;
#21645 = FACE_OUTER_BOUND ( 'NONE', #1453, .T. ) ;
#21646 = PRODUCT_DEFINITION_SHAPE ( 'NONE', 'NONE',  #23826 ) ;
#21647 = EDGE_CURVE ( 'NONE', #19218, #15819, #8007, .T. ) ;
#21649 = EDGE_LOOP ( 'NONE', ( #12688, #13262, #12905, #4346 ) ) ;
#21648 = ORIENTED_EDGE ( 'NONE', *, *, #20877, .T. ) ;
#21650 = DIRECTION ( 'NONE',  ( 1.000000000000000000, 2.832769448823979947E-16, -2.832769448823989808E-16 ) ) ;
#21651 = LINE ( 'NONE', #9089, #4243 ) ;
#21652 = CARTESIAN_POINT ( 'NONE',  ( 99.99999999999987210, -132.1999999999993634, 147.2000000000013813 ) ) ;
#21653 = DIRECTION ( 'NONE',  ( 1.000000000000000000, -3.051161311199799893E-31, -8.144298233840332611E-17 ) ) ;
#21654 = LINE ( 'NONE', #19831, #11478 ) ;
#21655 = ORIENTED_EDGE ( 'NONE', *, *, #19525, .T. ) ;
#21656 = DIRECTION ( 'NONE',  ( -1.000000000000000000, -5.478074134663600261E-16, 0.000000000000000000 ) ) ;
#21657 = ORIENTED_EDGE ( 'NONE', *, *, #23003, .T. ) ;
#21658 = DIRECTION ( 'NONE',  ( -1.000000000000000000, 0.000000000000000000, 0.000000000000000000 ) ) ;
#21659 = FACE_BOUND ( 'NONE', #10669, .T. ) ;
#21660 = ORIENTED_EDGE ( 'NONE', *, *, #5467, .F. ) ;
#21661 = ORIENTED_EDGE ( 'NONE', *, *, #2944, .T. ) ;
#21662 = CARTESIAN_POINT ( 'NONE',  ( -128.0900118278588877, 87.28149574061879434, -32.49999999999351985 ) ) ;
#21663 = CARTESIAN_POINT ( 'NONE',  ( 80.00000000000004263, -137.9999999999999716, 3.000000000000000000 ) ) ;
#21664 = ORIENTED_EDGE ( 'NONE', *, *, #11595, .F. ) ;
#21665 = CARTESIAN_POINT ( 'NONE',  ( -280.9020829022175576, 270.8299054689547347, 149.2295083325148539 ) ) ;
#21666 = DIRECTION ( 'NONE',  ( 1.000000000000000000, 0.000000000000000000, 0.000000000000000000 ) ) ;
#21667 = CARTESIAN_POINT ( 'NONE',  ( 93.00000000000000000, -149.9999999999996874, 129.9038105676659711 ) ) ;
#21668 = CARTESIAN_POINT ( 'NONE',  ( -64.99999999999995737, -56.79999999999964899, 65.00000000000018474 ) ) ;
#21669 = DIRECTION ( 'NONE',  ( 0.000000000000000000, 1.000000000000000000, 0.000000000000000000 ) ) ;
#21670 = CARTESIAN_POINT ( 'NONE',  ( -49.99999999999997158, -138.3994082814338071, -3.599999999999746070 ) ) ;
#21671 = CARTESIAN_POINT ( 'NONE',  ( 0.000000000000000000, 0.000000000000000000, 3.000000000000000000 ) ) ;
#21672 = VERTEX_POINT ( 'NONE', #10920 ) ;
#21673 = EDGE_CURVE ( 'NONE', #19527, #14436, #3743, .T. ) ;
#21674 = ITEM_DEFINED_TRANSFORMATION ( 'NONE', 'NONE', #10045,  #11210 ) ;
#21675 = CARTESIAN_POINT ( 'NONE',  ( -7.500000000000000000, -3.469446951953614189E-15, -6.991905250253751980 ) ) ;
#21676 = FACE_OUTER_BOUND ( 'NONE', #6420, .T. ) ;
#21677 = EDGE_CURVE ( 'NONE', #21251, #223, #23570, .T. ) ;
#21678 = ORIENTED_EDGE ( 'NONE', *, *, #17010, .F. ) ;
#21679 = DIRECTION ( 'NONE',  ( 6.982962677686266711E-15, -9.837870180509810443E-29, 1.000000000000000000 ) ) ;
#21680 = CARTESIAN_POINT ( 'NONE',  ( 0.000000000000000000, 0.000000000000000000, -150.0000000000000000 ) ) ;
#21681 = ADVANCED_FACE ( 'NONE', ( #12625 ), #16567, .T. ) ;
#21682 = EDGE_CURVE ( 'NONE', #5008, #15114, #14199, .T. ) ;
#21683 = AXIS2_PLACEMENT_3D ( 'NONE', #20358, #15089, #3826 ) ;
#21684 = CARTESIAN_POINT ( 'NONE',  ( -280.2840560642351875, 269.9696999999999889, 145.1244266425809712 ) ) ;
#21685 = DIRECTION ( 'NONE',  ( -0.000000000000000000, 0.000000000000000000, 1.000000000000000000 ) ) ;
#21686 = CARTESIAN_POINT ( 'NONE',  ( -284.9329465209281125, 269.4795879751482630, -146.1810844504667557 ) ) ;
#21687 = ORIENTED_EDGE ( 'NONE', *, *, #1850, .F. ) ;
#21688 = FACE_OUTER_BOUND ( 'NONE', #17723, .T. ) ;
#21689 = EDGE_LOOP ( 'NONE', ( #5065, #17294, #18609, #16923 ) ) ;
#21690 = FACE_OUTER_BOUND ( 'NONE', #12168, .T. ) ;
#21692 = EDGE_CURVE ( 'NONE', #18517, #19974, #9083, .T. ) ;
#21691 = DIRECTION ( 'NONE',  ( 0.000000000000000000, 1.000000000000000000, 4.183096374613631247E-18 ) ) ;
#21693 = FACE_OUTER_BOUND ( 'NONE', #21953, .T. ) ;
#21694 = ORIENTED_EDGE ( 'NONE', *, *, #6704, .T. ) ;
#21695 = CARTESIAN_POINT ( 'NONE',  ( -145.0000000000000284, -999.9999999999998863, -90.00000000000000000 ) ) ;
#21696 = DIRECTION ( 'NONE',  ( -1.000000000000000000, -0.000000000000000000, -0.000000000000000000 ) ) ;
#21697 = DIRECTION ( 'NONE',  ( 0.000000000000000000, 0.000000000000000000, 1.000000000000000000 ) ) ;
#21698 = CARTESIAN_POINT ( 'NONE',  ( 194.7500000000002274, -801.0618695410406644, -32.49999999999322853 ) ) ;
#21699 = DIRECTION ( 'NONE',  ( 0.000000000000000000, 0.000000000000000000, -1.000000000000000000 ) ) ;
#21700 = CARTESIAN_POINT ( 'NONE',  ( 2.500000000000000000, 0.000000000000000000, 0.000000000000000000 ) ) ;
#21701 = VECTOR ( 'NONE', #5304, 1000.000000000000000 ) ;
#21702 = ORIENTED_EDGE ( 'NONE', *, *, #18259, .T. ) ;
#21703 = ORIENTED_EDGE ( 'NONE', *, *, #5286, .F. ) ;
#21704 = DIRECTION ( 'NONE',  ( 1.000000000000000000, 0.000000000000000000, 0.000000000000000000 ) ) ;
#21705 = CARTESIAN_POINT ( 'NONE',  ( 5.200000000000002842, 0.000000000000000000, 0.000000000000000000 ) ) ;
#21706 = ORIENTED_EDGE ( 'NONE', *, *, #16669, .T. ) ;
#21707 = CARTESIAN_POINT ( 'NONE',  ( 5.200000000000002842, 0.000000000000000000, 0.000000000000000000 ) ) ;
#21708 = DIRECTION ( 'NONE',  ( -1.000000000000000000, -3.469446951953612710E-16, 5.618537574014070918E-17 ) ) ;
#21709 = ADVANCED_FACE ( 'NONE', ( #21645 ), #5101, .F. ) ;
#21710 = ORIENTED_EDGE ( 'NONE', *, *, #19409, .T. ) ;
#21711 = DIRECTION ( 'NONE',  ( 0.000000000000000000, -2.618450529776313049E-15, -1.000000000000000000 ) ) ;
#21712 = EDGE_CURVE ( 'NONE', #14084, #1754, #12511, .T. ) ;
#21713 = DIRECTION ( 'NONE',  ( 1.000000000000000000, 0.000000000000000000, 0.000000000000000000 ) ) ;
#21714 = ORIENTED_EDGE ( 'NONE', *, *, #11972, .T. ) ;
#21715 = ADVANCED_FACE ( 'NONE', ( #19937 ), #3614, .F. ) ;
#21716 = FACE_OUTER_BOUND ( 'NONE', #21477, .T. ) ;
#21717 = CIRCLE ( 'NONE', #13679, 0.7733184030943203169 ) ;
#21718 = ADVANCED_FACE ( 'NONE', ( #14416 ), #3388, .F. ) ;
#21719 = ORIENTED_EDGE ( 'NONE', *, *, #14182, .T. ) ;
#21720 = LINE ( 'NONE', #5178, #18037 ) ;
#21721 = PRODUCT_RELATED_PRODUCT_CATEGORY ( 'part', '', ( #6496 ) ) ;
#21722 = CARTESIAN_POINT ( 'NONE',  ( -42.98333333333332007, -89.99999999999997158, 3.000000000000001332 ) ) ;
#21723 = ADVANCED_FACE ( 'NONE', ( #2300 ), #9950, .F. ) ;
#21724 = CARTESIAN_POINT ( 'NONE',  ( -4.174999999999999822, 5.112900386440199535E-16, -0.5776712190230133270 ) ) ;
#21725 = ORIENTED_EDGE ( 'NONE', *, *, #1679, .F. ) ;
#21726 = ORIENTED_EDGE ( 'NONE', *, *, #843, .T. ) ;
#21727 = LINE ( 'NONE', #23045, #15812 ) ;
#21728 = DIRECTION ( 'NONE',  ( 0.1064154817287535221, 0.9943217513704692978, 1.303213790788408974E-17 ) ) ;
#21729 = CARTESIAN_POINT ( 'NONE',  ( -127.5331898753157276, 88.09262935741099909, -32.42132972170175265 ) ) ;
#21730 = CARTESIAN_POINT ( 'NONE',  ( 24.99999999999998224, -1000.000000000000000, -145.0000060000000417 ) ) ;
#21731 = CARTESIAN_POINT ( 'NONE',  ( 3.999999999999999112, -0.3979232138631231819, -5.929230630780099908E-17 ) ) ;
#21732 = AXIS2_PLACEMENT_3D ( 'NONE', #4878, #23, #8517 ) ;
#21733 = COLOUR_RGB ( '',0.8941176470588234615, 0.8941176470588234615, 0.8941176470588234615 ) ;
#21734 = ORIENTED_EDGE ( 'NONE', *, *, #4041, .T. ) ;
#21735 = DIRECTION ( 'NONE',  ( -0.000000000000000000, 0.000000000000000000, 1.000000000000000000 ) ) ;
#21736 = ORIENTED_EDGE ( 'NONE', *, *, #6971, .T. ) ;
#21737 = DIRECTION ( 'NONE',  ( 0.000000000000000000, 0.000000000000000000, -1.000000000000000000 ) ) ;
#21738 = CARTESIAN_POINT ( 'NONE',  ( 112.7436279071538792, -91.18044947428830937, -2.775557561562891351E-14 ) ) ;
#21739 = VERTEX_POINT ( 'NONE', #20409 ) ;
#21740 = CARTESIAN_POINT ( 'NONE',  ( -56.99999999999995737, -62.00000000000001421, 5.199999999999997513 ) ) ;
#21741 = AXIS2_PLACEMENT_3D ( 'NONE', #6393, #15836, #4581 ) ;
#21742 = ORIENTED_EDGE ( 'NONE', *, *, #18454, .T. ) ;
#21743 = CIRCLE ( 'NONE', #22888, 4.250000000000000000 ) ;
#21744 = EDGE_CURVE ( 'NONE', #7697, #4863, #21879, .T. ) ;
#21745 = ADVANCED_FACE ( 'NONE', ( #22578 ), #23422, .T. ) ;
#21746 = FACE_OUTER_BOUND ( 'NONE', #11921, .T. ) ;
#21747 = ADVANCED_FACE ( 'NONE', ( #20645, #502, #11511, #139, #18707, #3873, #7752, #4100, #14881, #22214 ), #9805, .F. ) ;
#21748 = ORIENTED_EDGE ( 'NONE', *, *, #15881, .T. ) ;
#21749 = DIRECTION ( 'NONE',  ( -0.000000000000000000, -0.000000000000000000, 1.000000000000000000 ) ) ;
#21750 = DIRECTION ( 'NONE',  ( 0.000000000000000000, 0.000000000000000000, -1.000000000000000000 ) ) ;
#21751 = DIRECTION ( 'NONE',  ( -0.000000000000000000, -0.000000000000000000, 1.000000000000000000 ) ) ;
#21752 = DIRECTION ( 'NONE',  ( 0.000000000000000000, 0.000000000000000000, 1.000000000000000000 ) ) ;
#21753 = ORIENTED_EDGE ( 'NONE', *, *, #10824, .T. ) ;
#21754 = LINE ( 'NONE', #18242, #18114 ) ;
#21755 = VECTOR ( 'NONE', #104, 1000.000000000000114 ) ;
#21757 = ORIENTED_EDGE ( 'NONE', *, *, #17276, .F. ) ;
#21756 = EDGE_LOOP ( 'NONE', ( #21448, #11658, #9175, #2865 ) ) ;
#21758 = AXIS2_PLACEMENT_3D ( 'NONE', #21200, #19007, #2474 ) ;
#21759 = CARTESIAN_POINT ( 'NONE',  ( 45.00000000000001421, -47.79999999999935056, 340.0000000000001705 ) ) ;
#21760 = CARTESIAN_POINT ( 'NONE',  ( 119.9257125005558606, -1087.686723660049893, 32.50000000000641620 ) ) ;
#21761 = DIRECTION ( 'NONE',  ( -1.000000000000000000, 0.000000000000000000, 0.000000000000000000 ) ) ;
#21762 = AXIS2_PLACEMENT_3D ( 'NONE', #2145, #4078, #19050 ) ;
#21763 = ORIENTED_EDGE ( 'NONE', *, *, #20041, .F. ) ;
#21764 = CYLINDRICAL_SURFACE ( 'NONE', #21085, 20.00000000000000000 ) ;
#21765 = VERTEX_POINT ( 'NONE', #9332 ) ;
#21766 = DIRECTION ( 'NONE',  ( 1.000000000000000000, 0.000000000000000000, 0.000000000000000000 ) ) ;
#21767 = VERTEX_POINT ( 'NONE', #5684 ) ;
#21768 = DIRECTION ( 'NONE',  ( 1.000000000000000000, 0.000000000000000000, 0.000000000000000000 ) ) ;
#21769 = CARTESIAN_POINT ( 'NONE',  ( 20.55500000000001748, 0.000000000000000000, 2.500000000000000888 ) ) ;
#21770 = VERTEX_POINT ( 'NONE', #18828 ) ;
#21771 = ORIENTED_EDGE ( 'NONE', *, *, #3963, .T. ) ;
#21772 = AXIS2_PLACEMENT_3D ( 'NONE', #1368, #15890, #6808 ) ;
#21773 = CARTESIAN_POINT ( 'NONE',  ( -24.99999999999998579, -37.41657386773942306, 125.0000000000001705 ) ) ;
#21774 = ORIENTED_EDGE ( 'NONE', *, *, #11892, .T. ) ;
#21775 = SURFACE_STYLE_USAGE ( .BOTH. , #12425 ) ;
#21776 = DIRECTION ( 'NONE',  ( 0.000000000000000000, 0.000000000000000000, 1.000000000000000000 ) ) ;
#21777 = VECTOR ( 'NONE', #15967, 1000.000000000000000 ) ;
#21778 = LINE ( 'NONE', #3533, #13094 ) ;
#21779 = VECTOR ( 'NONE', #15613, 1000.000000000000000 ) ;
#21780 = CARTESIAN_POINT ( 'NONE',  ( 67.35000000000002274, -112.6666666666666714, 124.9999999999999858 ) ) ;
#21781 = DIRECTION ( 'NONE',  ( -1.000000000000000000, 3.495664435217746592E-15, -0.000000000000000000 ) ) ;
#21782 = DIRECTION ( 'NONE',  ( 1.000000000000000000, 0.000000000000000000, 0.000000000000000000 ) ) ;
#21783 = ORIENTED_EDGE ( 'NONE', *, *, #4305, .F. ) ;
#21784 = LINE ( 'NONE', #16471, #22269 ) ;
#21785 = CARTESIAN_POINT ( 'NONE',  ( -4.236525694536558362, 2.416953475386465211, -3.751298745799836354 ) ) ;
#21786 = ORIENTED_EDGE ( 'NONE', *, *, #7623, .F. ) ;
#21787 = AXIS2_PLACEMENT_3D ( 'NONE', #18211, #13052, #20132 ) ;
#21788 = DIRECTION ( 'NONE',  ( 0.000000000000000000, -0.000000000000000000, 1.000000000000000000 ) ) ;
#21789 = CARTESIAN_POINT ( 'NONE',  ( 0.000000000000000000, 2.357898499370431722, -2.818925648462311528E-15 ) ) ;
#21790 = EDGE_CURVE ( 'NONE', #10284, #15178, #11283, .T. ) ;
#21791 = CARTESIAN_POINT ( 'NONE',  ( -284.5699028110928452, 270.4339272673396977, 145.9952621458756425 ) ) ;
#21792 = VECTOR ( 'NONE', #16732, 1000.000000000000000 ) ;
#21793 = DIRECTION ( 'NONE',  ( 1.000000000000000000, 0.000000000000000000, 0.000000000000000000 ) ) ;
#21794 = CARTESIAN_POINT ( 'NONE',  ( 0.000000000000000000, 0.000000000000000000, 0.000000000000000000 ) ) ;
#21795 = EDGE_LOOP ( 'NONE', ( #17774, #22548, #18217, #14296 ) ) ;
#21796 = CARTESIAN_POINT ( 'NONE',  ( 0.000000000000000000, 0.000000000000000000, -5.000000000000000000 ) ) ;
#21797 = ORIENTED_EDGE ( 'NONE', *, *, #9440, .F. ) ;
#21798 = ADVANCED_FACE ( 'NONE', ( #2167 ), #13455, .F. ) ;
#21799 = LINE ( 'NONE', #12670, #7545 ) ;
#21800 = PLANE ( 'NONE',  #7726 ) ;
#21801 = VECTOR ( 'NONE', #4612, 1000.000000000000000 ) ;
#21802 = EDGE_CURVE ( 'NONE', #10087, #20023, #13332, .T. ) ;
#21803 = ORIENTED_EDGE ( 'NONE', *, *, #8004, .T. ) ;
#21804 =( NAMED_UNIT ( * ) PLANE_ANGLE_UNIT ( ) SI_UNIT ( $, .RADIAN. ) );
#21805 = DIRECTION ( 'NONE',  ( 1.000000000000000000, -0.000000000000000000, -0.000000000000000000 ) ) ;
#21806 = CARTESIAN_POINT ( 'NONE',  ( 155.0000000000000284, 2.775557561562891351E-16, 90.00000000000000000 ) ) ;
#21807 = PLANE ( 'NONE',  #17504 ) ;
#21808 = CARTESIAN_POINT ( 'NONE',  ( 5.000000000000015099, 5.204748896376250699E-16, -4.250000000000000000 ) ) ;
#21809 = ADVANCED_FACE ( 'NONE', ( #7492 ), #1942, .F. ) ;
#21810 = DIRECTION ( 'NONE',  ( 0.000000000000000000, 0.000000000000000000, 1.000000000000000000 ) ) ;
#21811 = LINE ( 'NONE', #10740, #6289 ) ;
#21812 = AXIS2_PLACEMENT_3D ( 'NONE', #19846, #19473, #1004 ) ;
#21813 = ORIENTED_EDGE ( 'NONE', *, *, #15508, .T. ) ;
#21814 = ORIENTED_EDGE ( 'NONE', *, *, #17835, .T. ) ;
#21815 = LINE ( 'NONE', #14829, #17260 ) ;
#21816 = CARTESIAN_POINT ( 'NONE',  ( -281.4928932188135491, -132.2000000000000455, 7.703011046602857601E-15 ) ) ;
#21817 = EDGE_LOOP ( 'NONE', ( #8194, #1549, #6074 ) ) ;
#21818 = CARTESIAN_POINT ( 'NONE',  ( -20.00000000000000000, 2.449293598294706513E-15, 200.0000000000000000 ) ) ;
#21819 = DIRECTION ( 'NONE',  ( -1.350636282998972974E-14, 0.000000000000000000, -1.000000000000000000 ) ) ;
#21820 = AXIS2_PLACEMENT_3D ( 'NONE', #20329, #3788, #11692 ) ;
#21821 = ORIENTED_EDGE ( 'NONE', *, *, #7257, .T. ) ;
#21822 = CARTESIAN_POINT ( 'NONE',  ( 281.2440776823444253, 269.1689414351989740, 150.0938770989752982 ) ) ;
#21823 = CARTESIAN_POINT ( 'NONE',  ( -130.4031948627971076, -44.80746418436799416, 90.00000000000000000 ) ) ;
#21824 = VERTEX_POINT ( 'NONE', #253 ) ;
#21825 = CARTESIAN_POINT ( 'NONE',  ( 24.33333333333333215, -89.99999999999998579, 3.000000000000001332 ) ) ;
#21826 = VERTEX_POINT ( 'NONE', #15004 ) ;
#21827 = DIRECTION ( 'NONE',  ( 0.000000000000000000, -2.618450529776326854E-15, -1.000000000000000000 ) ) ;
#21828 = LINE ( 'NONE', #14731, #12906 ) ;
#21829 = ORIENTED_EDGE ( 'NONE', *, *, #17842, .F. ) ;
#21830 = ORIENTED_EDGE ( 'NONE', *, *, #18138, .F. ) ;
#21831 = DIRECTION ( 'NONE',  ( -0.000000000000000000, -0.000000000000000000, 1.000000000000000000 ) ) ;
#21832 = CARTESIAN_POINT ( 'NONE',  ( -126.6510233831467929, 89.35617925171790432, -28.74099766568598824 ) ) ;
#21833 = EDGE_CURVE ( 'NONE', #19773, #20258, #19953, .T. ) ;
#21834 = DIRECTION ( 'NONE',  ( 0.9289202219288174023, 0.3702799228849934510, 6.982962677686266711E-15 ) ) ;
#21835 = VERTEX_POINT ( 'NONE', #18617 ) ;
#21836 = CYLINDRICAL_SURFACE ( 'NONE', #10556, 7.500000000000007105 ) ;
#21837 = EDGE_CURVE ( 'NONE', #17692, #23165, #16477, .T. ) ;
#21838 = ORIENTED_EDGE ( 'NONE', *, *, #20658, .T. ) ;
#21839 = AXIS2_PLACEMENT_3D ( 'NONE', #23498, #9007, #16371 ) ;
#21840 = CARTESIAN_POINT ( 'NONE',  ( 11.07878015919985870, -22.47082401081930314, 145.0000119999999697 ) ) ;
#21841 =( NAMED_UNIT ( * ) PLANE_ANGLE_UNIT ( ) SI_UNIT ( $, .RADIAN. ) );
#21842 = EDGE_CURVE ( 'NONE', #16311, #1754, #10890, .T. ) ;
#21843 = EDGE_CURVE ( 'NONE', #6345, #16779, #14729, .T. ) ;
#21844 = CIRCLE ( 'NONE', #18765, 5.249999999999949374 ) ;
#21845 = CARTESIAN_POINT ( 'NONE',  ( -146.0000000000000853, -784.4690652294805204, 30.00000000000641620 ) ) ;
#21846 = CARTESIAN_POINT ( 'NONE',  ( -282.2000000000007276, 75.00000000000098055, 90.00000000000000000 ) ) ;
#21847 = ORIENTED_EDGE ( 'NONE', *, *, #10221, .F. ) ;
#21848 = VECTOR ( 'NONE', #8829, 1000.000000000000114 ) ;
#21849 = CARTESIAN_POINT ( 'NONE',  ( 312.2000000000013529, -132.2000000000000455, -146.4928932188134070 ) ) ;
#21850 = EDGE_LOOP ( 'NONE', ( #9169, #13277, #2237, #6695 ) ) ;
#21851 = CARTESIAN_POINT ( 'NONE',  ( 4.000000000000000000, -2.309401076758514915, -5.000000000000000000 ) ) ;
#21852 = ORIENTED_EDGE ( 'NONE', *, *, #15980, .T. ) ;
#21853 = CYLINDRICAL_SURFACE ( 'NONE', #1545, 2.649999999999971934 ) ;
#21854 = EDGE_CURVE ( 'NONE', #2150, #23797, #2209, .T. ) ;
#21855 = CARTESIAN_POINT ( 'NONE',  ( -24.20041621714723235, -1006.482064212727892, 145.0000119999999413 ) ) ;
#21856 = AXIS2_PLACEMENT_3D ( 'NONE', #22348, #12540, #13224 ) ;
#21857 = CARTESIAN_POINT ( 'NONE',  ( 2.500000000000000000, 1.178949249685213863, -2.042000000000001148 ) ) ;
#21858 = DIRECTION ( 'NONE',  ( 0.000000000000000000, 0.000000000000000000, 1.000000000000000000 ) ) ;
#21859 = DIRECTION ( 'NONE',  ( -1.000000000000000000, -0.000000000000000000, -0.000000000000000000 ) ) ;
#21860 = VERTEX_POINT ( 'NONE', #3829 ) ;
#21861 = DIRECTION ( 'NONE',  ( 0.000000000000000000, -1.110223024625156540E-16, 1.000000000000000000 ) ) ;
#21862 = AXIS2_PLACEMENT_3D ( 'NONE', #5547, #3720, #1920 ) ;
#21863 = AXIS2_PLACEMENT_3D ( 'NONE', #16919, #9295, #16301 ) ;
#21865 = EDGE_LOOP ( 'NONE', ( #1593, #7017 ) ) ;
#21864 = ORIENTED_EDGE ( 'NONE', *, *, #619, .T. ) ;
#21866 = DIRECTION ( 'NONE',  ( 1.221966984364620947E-29, 3.495664435217746987E-15, -1.000000000000000000 ) ) ;
#21867 = EDGE_CURVE ( 'NONE', #1352, #160, #1048, .T. ) ;
#21868 = DIRECTION ( 'NONE',  ( 0.000000000000000000, 1.224646799147346305E-16, 1.000000000000000000 ) ) ;
#21869 = LINE ( 'NONE', #21652, #23438 ) ;
#21870 = EDGE_CURVE ( 'NONE', #11281, #20963, #2970, .T. ) ;
#21871 = VERTEX_POINT ( 'NONE', #1895 ) ;
#21872 = CARTESIAN_POINT ( 'NONE',  ( -20.63749999999999929, 0.000000000000000000, 0.000000000000000000 ) ) ;
#21873 = VECTOR ( 'NONE', #12465, 1000.000000000000000 ) ;
#21874 = DIRECTION ( 'NONE',  ( 1.000000000000000000, 0.000000000000000000, 0.000000000000000000 ) ) ;
#21875 = VERTEX_POINT ( 'NONE', #20364 ) ;
#21876 = VECTOR ( 'NONE', #6685, 1000.000000000000000 ) ;
#21877 = DIRECTION ( 'NONE',  ( -6.982962677686266711E-15, 0.000000000000000000, 1.000000000000000000 ) ) ;
#21878 = DIRECTION ( 'NONE',  ( -1.000000000000000000, 1.408839003528726857E-14, 6.982962677686266711E-15 ) ) ;
#21879 = CIRCLE ( 'NONE', #5311, 2.649999999999985700 ) ;
#21880 = VERTEX_POINT ( 'NONE', #5294 ) ;
#21881 = CIRCLE ( 'NONE', #3778, 24.99999999999998224 ) ;
#21882 = VERTEX_POINT ( 'NONE', #16650 ) ;
#21883 = LINE ( 'NONE', #16461, #22581 ) ;
#21884 = ORIENTED_EDGE ( 'NONE', *, *, #4904, .F. ) ;
#21885 =( LENGTH_UNIT ( ) NAMED_UNIT ( * ) SI_UNIT ( .MILLI., .METRE. ) );
#21886 = DIRECTION ( 'NONE',  ( 0.3090169943749589421, -0.9510565162951498674, 0.000000000000000000 ) ) ;
#21887 = DIRECTION ( 'NONE',  ( -1.000000000000000000, 3.495664435217746987E-15, 0.000000000000000000 ) ) ;
#21888 = CARTESIAN_POINT ( 'NONE',  ( 34.99999999999999289, 0.000000000000000000, 0.000000000000000000 ) ) ;
#21889 = CYLINDRICAL_SURFACE ( 'NONE', #20394, 2.200000000000028155 ) ;
#21890 = AXIS2_PLACEMENT_3D ( 'NONE', #13531, #8054, #22410 ) ;
#21891 = ORIENTED_EDGE ( 'NONE', *, *, #7102, .T. ) ;
#21892 = DIRECTION ( 'NONE',  ( 1.000000000000000000, 0.000000000000000000, 0.000000000000000000 ) ) ;
#21893 = EDGE_CURVE ( 'NONE', #1699, #12610, #16522, .T. ) ;
#21894 = DIRECTION ( 'NONE',  ( 0.000000000000000000, 0.000000000000000000, 1.000000000000000000 ) ) ;
#21895 = CIRCLE ( 'NONE', #20743, 2.649999999999985700 ) ;
#21896 = DIRECTION ( 'NONE',  ( 0.000000000000000000, 0.000000000000000000, -1.000000000000000000 ) ) ;
#21897 = CIRCLE ( 'NONE', #14983, 145.0000000000000284 ) ;
#21898 = ORIENTED_EDGE ( 'NONE', *, *, #10672, .F. ) ;
#21899 = VECTOR ( 'NONE', #14349, 1000.000000000000000 ) ;
#21900 = EDGE_CURVE ( 'NONE', #15535, #7773, #3352, .T. ) ;
#21901 = CARTESIAN_POINT ( 'NONE',  ( 2.500000000000015987, -1.768423874527823347, -1.020999999999997687 ) ) ;
#21902 = DIRECTION ( 'NONE',  ( 5.618537574013950123E-17, 3.483493295888648978E-15, 1.000000000000000000 ) ) ;
#21903 = CARTESIAN_POINT ( 'NONE',  ( -281.1079617568159961, 269.7223300543793698, 145.4976310729378213 ) ) ;
#21904 = LINE ( 'NONE', #5381, #3323 ) ;
#21905 = CARTESIAN_POINT ( 'NONE',  ( 280.3120962995436116, 272.7324007871372373, -146.6810649015076535 ) ) ;
#21906 = VERTEX_POINT ( 'NONE', #22177 ) ;
#21907 = CARTESIAN_POINT ( 'NONE',  ( 5.000000000000000000, -2.342598717236910488, -4.057499999999997442 ) ) ;
#21908 = ORIENTED_EDGE ( 'NONE', *, *, #14537, .F. ) ;
#21910 = CARTESIAN_POINT ( 'NONE',  ( -146.4450000000000500, -784.4690652294805204, 32.50000000000641620 ) ) ;
#21909 = VECTOR ( 'NONE', #23253, 1000.000000000000000 ) ;
#21911 = CIRCLE ( 'NONE', #4182, 4.000000000000000000 ) ;
#21912 = AXIS2_PLACEMENT_3D ( 'NONE', #12490, #21834, #14396 ) ;
#21913 = ORIENTED_EDGE ( 'NONE', *, *, #7984, .F. ) ;
#21914 = CARTESIAN_POINT ( 'NONE',  ( 25.00000000000001066, 45.00100000000043821, 64.99999999999984368 ) ) ;
#21915 = AXIS2_PLACEMENT_3D ( 'NONE', #21512, #23675, #1589 ) ;
#21916 = CARTESIAN_POINT ( 'NONE',  ( 122.9460700935424171, -1094.388896850127367, -30.32927184981470958 ) ) ;
#21917 = CARTESIAN_POINT ( 'NONE',  ( 0.000000000000000000, -132.2000000000000455, 177.2000000000014097 ) ) ;
#21918 = CARTESIAN_POINT ( 'NONE',  ( -288.2000000000011255, -29.99999999999898037, -107.6499999999999631 ) ) ;
#21919 = DIRECTION ( 'NONE',  ( 1.000000000000000000, -3.495664435217746987E-15, -0.000000000000000000 ) ) ;
#21920 = CARTESIAN_POINT ( 'NONE',  ( -4.000000000000000000, -2.309401076758515803, -0.4999999999999995559 ) ) ;
#21921 = CIRCLE ( 'NONE', #10396, 35.00000000000000711 ) ;
#21922 = ADVANCED_FACE ( 'NONE', ( #14845 ), #14490, .F. ) ;
#21923 = CARTESIAN_POINT ( 'NONE',  ( -18.83467029480912203, 16.52066876451825550, 145.0000119999999697 ) ) ;
#21924 = EDGE_LOOP ( 'NONE', ( #13856, #17231, #17237, #7889 ) ) ;
#21925 = ORIENTED_EDGE ( 'NONE', *, *, #23613, .T. ) ;
#21926 = PLANE ( 'NONE',  #4530 ) ;
#21927 = FACE_OUTER_BOUND ( 'NONE', #1713, .T. ) ;
#21928 = EDGE_LOOP ( 'NONE', ( #6824, #20748, #12577, #4946 ) ) ;
#21929 = EDGE_CURVE ( 'NONE', #14713, #18285, #3104, .T. ) ;
#21930 = B_SPLINE_SURFACE_WITH_KNOTS ( 'NONE', 1, 3, ( 
 ( #12445, #19864, #7303, #19744, #5490, #1734, #21791, #16264, #3314, #1625 ),
 ( #8774, #16022, #3549, #10721, #18061, #19977, #18280, #7173, #9124, #16479 ),
 ( #15462, #6961, #12800, #21903, #23606, #20102, #14351, #14695, #12902, #7065 ),
 ( #10490, #21684, #17942, #8649, #3436, #6828, #5378, #12664, #14230, #5139 ) ),
 .UNSPECIFIED., .F., .F., .F.,
 ( 2, 1, 1, 2 ),
 ( 4, 2, 2, 2, 4 ),
 ( -0.01000000000000000021, 0.000000000000000000, 1.000000000000000000, 1.010099999999999998 ),
 ( 0.000000000000000000, 0.2500000000000000000, 0.5000000000000000000, 0.7500000000000000000, 1.000000000000000000 ),
 .UNSPECIFIED. ) ;
#21931 = VECTOR ( 'NONE', #18637, 1000.000000000000000 ) ;
#21932 = LINE ( 'NONE', #10989, #13175 ) ;
#21933 = DIRECTION ( 'NONE',  ( 1.000000000000000000, 0.000000000000000000, 0.000000000000000000 ) ) ;
#21935 = VECTOR ( 'NONE', #18358, 1000.000000000000000 ) ;
#21934 =( GEOMETRIC_REPRESENTATION_CONTEXT ( 3 ) GLOBAL_UNCERTAINTY_ASSIGNED_CONTEXT ( ( #9183 ) ) GLOBAL_UNIT_ASSIGNED_CONTEXT ( ( #4533, #2481, #8179 ) ) REPRESENTATION_CONTEXT ( 'NONE', 'WORKASPACE' ) );
#21936 = VECTOR ( 'NONE', #6600, 1000.000000000000000 ) ;
#21937 = CIRCLE ( 'NONE', #1119, 2.199999999999979750 ) ;
#21938 = EDGE_LOOP ( 'NONE', ( #2666, #17125 ) ) ;
#21939 = CARTESIAN_POINT ( 'NONE',  ( -281.4928932188135491, -132.2000000000000455, 152.4000000000014268 ) ) ;
#21940 = VECTOR ( 'NONE', #9227, 1000.000000000000000 ) ;
#21941 = AXIS2_PLACEMENT_3D ( 'NONE', #19029, #2496, #9884 ) ;
#21942 = DIRECTION ( 'NONE',  ( 0.000000000000000000, 1.000000000000000000, 0.000000000000000000 ) ) ;
#21943 = ORIENTED_EDGE ( 'NONE', *, *, #10226, .T. ) ;
#21944 = CARTESIAN_POINT ( 'NONE',  ( -79.99999999999995737, -62.00000000000007816, -3.122502256758252770E-14 ) ) ;
#21945 = EDGE_CURVE ( 'NONE', #15324, #3965, #14386, .T. ) ;
#21946 = CARTESIAN_POINT ( 'NONE',  ( 281.4928932188134354, -127.0000000000000568, -147.2000000000013245 ) ) ;
#21947 = SHAPE_REPRESENTATION ( 'discharge spout', ( #11210 ), #22754 ) ;
#21948 = EDGE_LOOP ( 'NONE', ( #19435, #16482, #22132, #17514 ) ) ;
#21949 = LINE ( 'NONE', #12832, #295 ) ;
#21950 = CARTESIAN_POINT ( 'NONE',  ( -135.7895026000614678, -1074.740959209980247, 27.50000000000646239 ) ) ;
#21951 = LINE ( 'NONE', #1776, #11360 ) ;
#21952 = ORIENTED_EDGE ( 'NONE', *, *, #1972, .T. ) ;
#21953 = EDGE_LOOP ( 'NONE', ( #14859, #21008, #3603, #4449 ) ) ;
#21954 = CARTESIAN_POINT ( 'NONE',  ( -122.8605704798722087, 82.74225173005940803, -32.05499999999356220 ) ) ;
#21955 = SHAPE_DEFINITION_REPRESENTATION ( #21545, #6508 ) ;
#21956 = CARTESIAN_POINT ( 'NONE',  ( -126.4950807468199798, 89.57684269074619010, -30.66034227022098690 ) ) ;
#21957 = AXIS2_PLACEMENT_3D ( 'NONE', #22738, #19221, #4274 ) ;
#21959 = FACE_OUTER_BOUND ( 'NONE', #13077, .T. ) ;
#21958 = AXIS2_PLACEMENT_3D ( 'NONE', #19369, #15185, #7920 ) ;
#21960 = CIRCLE ( 'NONE', #12369, 4.000000000000000000 ) ;
#21961 = CARTESIAN_POINT ( 'NONE',  ( -2.059999999999998721, 2.522772406243545965E-16, -0.3080913168122742518 ) ) ;
#21962 = VECTOR ( 'NONE', #16481, 1000.000000000000000 ) ;
#21963 = VECTOR ( 'NONE', #18304, 1000.000000000000114 ) ;
#21964 = EDGE_LOOP ( 'NONE', ( #21996, #8286, #2176, #765, #7791, #7268 ) ) ;
#21965 = B_SPLINE_CURVE_WITH_KNOTS ( 'NONE', 3,
 ( #13220, #9551, #385, #13327, #20640, #11646, #18950, #17158, #615, #7977, #11759, #17280, #7425, #7659, #11214, #5734, #13155, #9262, #2214, #2096, #16622, #16979, #11080, #22034, #20213, #5496, #18286, #20460, #11436, #16728, #22262, #20108, #11324, #13024 ),
 .UNSPECIFIED., .F., .F.,
 ( 4, 2, 2, 2, 2, 2, 2, 2, 2, 2, 2, 2, 2, 2, 2, 2, 4 ),
 ( 0.000000000000000000, 0.03125000000000000000, 0.06250000000000000000, 0.09375000000000000000, 0.1250000000000000000, 0.1562500000000000000, 0.1875000000000000000, 0.2187500000000000000, 0.2500000000000000000, 0.2812500000000000000, 0.3125000000000000000, 0.3437500000000000000, 0.3750000000000000000, 0.4062500000000000000, 0.4375000000000000000, 0.4687500000000000000, 0.5000000000000000000 ),
 .UNSPECIFIED. ) ;
#21966 = DIRECTION ( 'NONE',  ( 1.000000000000000000, 0.000000000000000000, 0.000000000000000000 ) ) ;
#21967 = VECTOR ( 'NONE', #633, 1000.000000000000000 ) ;
#21968 = EDGE_CURVE ( 'NONE', #8807, #6345, #21720, .T. ) ;
#21969 = EDGE_CURVE ( 'NONE', #8692, #9373, #14564, .T. ) ;
#21970 = FACE_OUTER_BOUND ( 'NONE', #23665, .T. ) ;
#21971 = DIRECTION ( 'NONE',  ( 0.000000000000000000, 0.000000000000000000, 1.000000000000000000 ) ) ;
#21973=STYLED_ITEM('',(#23927),#19781);
#21972 = AXIS2_PLACEMENT_3D ( 'NONE', #10563, #17900, #2910 ) ;
#21974 = VERTEX_POINT ( 'NONE', #12708 ) ;
#21975 = CARTESIAN_POINT ( 'NONE',  ( 2.547548355748054857E-16, 8.895721644649732696, -7.917989418073286600 ) ) ;
#21976 = AXIS2_PLACEMENT_3D ( 'NONE', #10176, #17419, #18967 ) ;
#21977 = ADVANCED_FACE ( 'NONE', ( #1665 ), #7348, .F. ) ;
#21978 = AXIS2_PLACEMENT_3D ( 'NONE', #4385, #22963, #4507 ) ;
#21979 = CIRCLE ( 'NONE', #763, 23.50000000000000000 ) ;
#21980 = EDGE_CURVE ( 'NONE', #21875, #5970, #21469, .T. ) ;
#21981 = ORIENTED_EDGE ( 'NONE', *, *, #22749, .F. ) ;
#21982 = DIRECTION ( 'NONE',  ( 0.000000000000000000, -1.000000000000000000, 1.287488025362403787E-15 ) ) ;
#21983 = CARTESIAN_POINT ( 'NONE',  ( -2.836893136758495970, -3.208949435745868328, -3.505054077164885484 ) ) ;
#21984 = ORIENTED_EDGE ( 'NONE', *, *, #3731, .F. ) ;
#21985 = EDGE_CURVE ( 'NONE', #4934, #4706, #21949, .T. ) ;
#21986 = CARTESIAN_POINT ( 'NONE',  ( 1.144235203016666258, 3.958177651039090250, -0.09382832055445661235 ) ) ;
#21987 = LINE ( 'NONE', #20761, #22506 ) ;
#21988 = DIRECTION ( 'NONE',  ( 0.000000000000000000, 0.000000000000000000, 1.000000000000000000 ) ) ;
#21989 = CARTESIAN_POINT ( 'NONE',  ( 125.9551925347489316, -1090.334326554368999, -29.66799569545560189 ) ) ;
#21990 = DIRECTION ( 'NONE',  ( -0.000000000000000000, 0.4999999999999979461, -0.8660254037844397068 ) ) ;
#21991 = EDGE_LOOP ( 'NONE', ( #2769, #18886 ) ) ;
#21992 = CIRCLE ( 'NONE', #3382, 45.00000000000000711 ) ;
#21993 = DIRECTION ( 'NONE',  ( -1.000000000000000000, -0.000000000000000000, -0.000000000000000000 ) ) ;
#21994 = VECTOR ( 'NONE', #20680, 1000.000000000000000 ) ;
#21996 = ORIENTED_EDGE ( 'NONE', *, *, #32, .T. ) ;
#21995 = ORIENTED_EDGE ( 'NONE', *, *, #995, .F. ) ;
#21997 = DIRECTION ( 'NONE',  ( 0.9237280213470682178, 0.3830490080632377725, 1.131240564625405124E-16 ) ) ;
#21998 = DIRECTION ( 'NONE',  ( 1.000000000000000000, -6.640089860198304064E-16, -0.000000000000000000 ) ) ;
#21999 = DIRECTION ( 'NONE',  ( -1.000000000000000000, 0.000000000000000000, -0.000000000000000000 ) ) ;
#22000 = VERTEX_POINT ( 'NONE', #3584 ) ;
#22001 = LINE ( 'NONE', #8979, #6795 ) ;
#22002 = EDGE_CURVE ( 'NONE', #3203, #19239, #13833, .T. ) ;
#22003 = EDGE_CURVE ( 'NONE', #784, #6379, #5151, .T. ) ;
#22004 = DIRECTION ( 'NONE',  ( 0.000000000000000000, -2.618450529776326854E-15, -1.000000000000000000 ) ) ;
#22005 = EDGE_CURVE ( 'NONE', #16905, #15299, #12565, .T. ) ;
#22006 = ORIENTED_EDGE ( 'NONE', *, *, #12764, .F. ) ;
#22007 = EDGE_CURVE ( 'NONE', #14121, #6031, #12684, .T. ) ;
#22008 = CARTESIAN_POINT ( 'NONE',  ( -31.74999999999994316, 3.061616997868383634E-16, -2.500000000000000444 ) ) ;
#22009 = DIRECTION ( 'NONE',  ( 1.000000000000000000, 0.000000000000000000, 0.000000000000000000 ) ) ;
#22010 = ORIENTED_EDGE ( 'NONE', *, *, #4149, .F. ) ;
#22011 = ORIENTED_EDGE ( 'NONE', *, *, #16828, .F. ) ;
#22012 = EDGE_CURVE ( 'NONE', #2882, #6583, #15802, .T. ) ;
#22013 = DIRECTION ( 'NONE',  ( 1.000000000000000000, 0.000000000000000000, 0.000000000000000000 ) ) ;
#22014 = ORIENTED_EDGE ( 'NONE', *, *, #14539, .T. ) ;
#22015 = ADVANCED_FACE ( 'NONE', ( #10502 ), #4794, .T. ) ;
#22016 = CARTESIAN_POINT ( 'NONE',  ( 18.83879023463319058, -983.4833815101718528, -145.0000000000001421 ) ) ;
#22017 = PLANE ( 'NONE',  #9609 ) ;
#22018 = LINE ( 'NONE', #20305, #7647 ) ;
#22019 = DIRECTION ( 'NONE',  ( 0.9510565162951580831, -0.3090169943749334069, 0.000000000000000000 ) ) ;
#22020 = B_SPLINE_CURVE_WITH_KNOTS ( 'NONE', 3,
 ( #16853, #3678, #9271, #11227, #20117, #316 ),
 .UNSPECIFIED., .F., .F.,
 ( 4, 2, 4 ),
 ( 0.000000000000000000, 0.0002095117440854730670, 0.0004190234881709461339 ),
 .UNSPECIFIED. ) ;
#22021 = DIRECTION ( 'NONE',  ( 0.000000000000000000, 1.000000000000000000, -3.548298019043423769E-15 ) ) ;
#22022 = VERTEX_POINT ( 'NONE', #17590 ) ;
#22023 = DIRECTION ( 'NONE',  ( 0.000000000000000000, 0.000000000000000000, 1.000000000000000000 ) ) ;
#22024 = DIRECTION ( 'NONE',  ( 1.000000000000000000, 0.000000000000000000, 0.000000000000000000 ) ) ;
#22025 = DIRECTION ( 'NONE',  ( 0.000000000000000000, 0.000000000000000000, 1.000000000000000000 ) ) ;
#22026 =( REPRESENTATION_RELATIONSHIP ('NONE','NONE', #10127, #15622 ) REPRESENTATION_RELATIONSHIP_WITH_TRANSFORMATION ( #8077 )SHAPE_REPRESENTATION_RELATIONSHIP( ) );
#22027 = ORIENTED_EDGE ( 'NONE', *, *, #849, .F. ) ;
#22028 = CARTESIAN_POINT ( 'NONE',  ( 135.4018704341550574, 51.87806360044960741, 90.00000000000000000 ) ) ;
#22029 = CARTESIAN_POINT ( 'NONE',  ( 158.0000000000000284, -2.237095343400623696E-14, 57.00000000000024869 ) ) ;
#22030 = FACE_OUTER_BOUND ( 'NONE', #18120, .T. ) ;
#22031 = DIRECTION ( 'NONE',  ( 1.000000000000000000, 0.000000000000000000, 0.000000000000000000 ) ) ;
#22032 = LINE ( 'NONE', #16840, #7312 ) ;
#22033 = EDGE_LOOP ( 'NONE', ( #3583, #4942, #17488, #49 ) ) ;
#22034 = CARTESIAN_POINT ( 'NONE',  ( -15.24974479720505549, -980.1223093604608039, 145.0000119999999697 ) ) ;
#22035 = ORIENTED_EDGE ( 'NONE', *, *, #2894, .F. ) ;
#22036 = DIRECTION ( 'NONE',  ( 0.000000000000000000, 0.000000000000000000, 1.000000000000000000 ) ) ;
#22037 = ADVANCED_FACE ( 'NONE', ( #14123 ), #12329, .F. ) ;
#22038 = ADVANCED_FACE ( 'NONE', ( #17955 ), #19511, .T. ) ;
#22039 = CARTESIAN_POINT ( 'NONE',  ( -4.000000000000000000, -2.309401076758515803, -0.4999999999999995559 ) ) ;
#22040 = ORIENTED_EDGE ( 'NONE', *, *, #1762, .T. ) ;
#22041 = DIRECTION ( 'NONE',  ( 0.6964005597823107463, -0.7176533009294140397, 6.982962677686265922E-15 ) ) ;
#22042 = CARTESIAN_POINT ( 'NONE',  ( -155.0000000000000284, -784.4690652294805204, 32.50000000000648015 ) ) ;
#22043 = FACE_BOUND ( 'NONE', #3998, .T. ) ;
#22044 = CARTESIAN_POINT ( 'NONE',  ( 23.72528575886166990, -1008.050112875828518, -145.0000000000001421 ) ) ;
#22045 = DIRECTION ( 'NONE',  ( -0.5000000000000005551, 0.8660254037844383745, 0.000000000000000000 ) ) ;
#22046 = CARTESIAN_POINT ( 'NONE',  ( 2.500000000000000000, 2.357898499370431722, -2.818925648462311528E-15 ) ) ;
#22047 = DIRECTION ( 'NONE',  ( 1.000000000000000000, -9.769962616701377556E-15, 0.000000000000000000 ) ) ;
#22048 = ORIENTED_EDGE ( 'NONE', *, *, #14092, .T. ) ;
#22049 = ORIENTED_EDGE ( 'NONE', *, *, #4335, .T. ) ;
#22050 = CARTESIAN_POINT ( 'NONE',  ( 171.6502151485109664, 95.33502053007563859, 30.00000000000675726 ) ) ;
#22051 = CARTESIAN_POINT ( 'NONE',  ( 40.00000000000000000, 100.0000000000000000, 150.2000000000009550 ) ) ;
#22052 = ORIENTED_EDGE ( 'NONE', *, *, #15548, .T. ) ;
#22053 = DIRECTION ( 'NONE',  ( -0.9423651898111408132, -0.3345860861306287348, 6.982962677686266711E-15 ) ) ;
#22054 = DIRECTION ( 'NONE',  ( -0.000000000000000000, -0.000000000000000000, 1.000000000000000000 ) ) ;
#22055 = ORIENTED_EDGE ( 'NONE', *, *, #13946, .T. ) ;
#22056 = FACE_OUTER_BOUND ( 'NONE', #14554, .T. ) ;
#22057 = CARTESIAN_POINT ( 'NONE',  ( -105.0000000000000142, 30.00000000000001421, 0.000000000000000000 ) ) ;
#22058 = ORIENTED_EDGE ( 'NONE', *, *, #3633, .T. ) ;
#22059 = CARTESIAN_POINT ( 'NONE',  ( -146.0000000000000853, -494.4690652294807478, 30.00000000000641620 ) ) ;
#22060 = DIRECTION ( 'NONE',  ( 3.202566417187928841E-16, -1.000000000000000000, 3.469446951953614583E-15 ) ) ;
#22061 = LINE ( 'NONE', #16755, #14288 ) ;
#22062 = EDGE_LOOP ( 'NONE', ( #22790, #5533 ) ) ;
#22063 = CARTESIAN_POINT ( 'NONE',  ( -100.0000000000001137, -132.2000000000001592, -113.4834095219707848 ) ) ;
#22064 = CARTESIAN_POINT ( 'NONE',  ( -136.1024116720894881, -1074.169801158669543, 27.57867027829822604 ) ) ;
#22065 = DIRECTION ( 'NONE',  ( -0.000000000000000000, 1.000000000000000000, -3.469446951953613794E-15 ) ) ;
#22066 = EDGE_LOOP ( 'NONE', ( #11682, #19982, #8854, #663, #16413, #13610 ) ) ;
#22067 = VERTEX_POINT ( 'NONE', #5270 ) ;
#22068 = DIRECTION ( 'NONE',  ( -1.000000000000000000, 0.000000000000000000, 0.000000000000000000 ) ) ;
#22069 = VECTOR ( 'NONE', #14959, 1000.000000000000000 ) ;
#22070 = APPLICATION_PROTOCOL_DEFINITION ( 'draft international standard', 'automotive_design', 1998, #11742 ) ;
#22071 = CARTESIAN_POINT ( 'NONE',  ( -126.9537165176728166, 88.92563123478259968, -28.11073331261975028 ) ) ;
#22072 = PLANE ( 'NONE',  #13477 ) ;
#22073 = CARTESIAN_POINT ( 'NONE',  ( -194.7500000000004832, -494.4690652294794404, -29.99999999999322498 ) ) ;
#22074 = EDGE_LOOP ( 'NONE', ( #8075, #1282, #3588, #658 ) ) ;
#22075 = CARTESIAN_POINT ( 'NONE',  ( -24.99999999999999645, -1.636246173744688726, 145.0000119999999697 ) ) ;
#22076 = LINE ( 'NONE', #5546, #16750 ) ;
#22077 = DIRECTION ( 'NONE',  ( -0.000000000000000000, -0.000000000000000000, 1.000000000000000000 ) ) ;
#22078 = ORIENTED_EDGE ( 'NONE', *, *, #6506, .F. ) ;
#22079 = DIRECTION ( 'NONE',  ( 0.000000000000000000, 1.000000000000000000, -1.287488025362403787E-15 ) ) ;
#22080 = ORIENTED_EDGE ( 'NONE', *, *, #19227, .F. ) ;
#22081 = DIRECTION ( 'NONE',  ( 1.000000000000000000, 0.000000000000000000, 0.000000000000000000 ) ) ;
#22082 = DIRECTION ( 'NONE',  ( 1.000000000000000000, 0.000000000000000000, 0.000000000000000000 ) ) ;
#22083 = ORIENTED_EDGE ( 'NONE', *, *, #6097, .F. ) ;
#22084 = CARTESIAN_POINT ( 'NONE',  ( -6.602753909532903975, -5.319290460493544259, -7.792447862505333056 ) ) ;
#22085 = EDGE_CURVE ( 'NONE', #16256, #640, #18075, .T. ) ;
#22086 = CYLINDRICAL_SURFACE ( 'NONE', #12009, 5.249999999999973355 ) ;
#22087 = CARTESIAN_POINT ( 'NONE',  ( 24.83884780301425366, -1003.272451888078649, 145.0000119999999697 ) ) ;
#22088 = EDGE_CURVE ( 'NONE', #67, #21882, #2849, .T. ) ;
#22089 = ADVANCED_FACE ( 'NONE', ( #1404 ), #8662, .F. ) ;
#22090 = CARTESIAN_POINT ( 'NONE',  ( -281.7502846751312404, 269.1405375976306686, -145.8716261326569565 ) ) ;
#22091 = AXIS2_PLACEMENT_3D ( 'NONE', #1995, #17102, #18766 ) ;
#22092 = CARTESIAN_POINT ( 'NONE',  ( 125.1337793500214275, -1091.468903702554144, -32.24903484778815255 ) ) ;
#22093 = DIRECTION ( 'NONE',  ( 0.000000000000000000, 0.000000000000000000, 1.000000000000000000 ) ) ;
#22094 = VERTEX_POINT ( 'NONE', #21695 ) ;
#22095 = CARTESIAN_POINT ( 'NONE',  ( -122.8605704798723082, 82.74225173005861222, 30.00000000000641620 ) ) ;
#22096 = LINE ( 'NONE', #2168, #15585 ) ;
#22097 =( NAMED_UNIT ( * ) PLANE_ANGLE_UNIT ( ) SI_UNIT ( $, .RADIAN. ) );
#22098 = EDGE_CURVE ( 'NONE', #10971, #10033, #10373, .T. ) ;
#22100 = VERTEX_POINT ( 'NONE', #14009 ) ;
#22099 = VERTEX_POINT ( 'NONE', #7078 ) ;
#22101 = CARTESIAN_POINT ( 'NONE',  ( -45.00000000000000000, 283.0000000000000000, 0.000000000000000000 ) ) ;
#22102 = CARTESIAN_POINT ( 'NONE',  ( -136.9530201128895328, -1072.586991580760241, -29.34813586885360337 ) ) ;
#22103 = CARTESIAN_POINT ( 'NONE',  ( 280.6220388411722411, 269.5350371479513001, -146.3333820183295302 ) ) ;
#22104 = ORIENTED_EDGE ( 'NONE', *, *, #10106, .F. ) ;
#22105 = AXIS2_PLACEMENT_3D ( 'NONE', #13928, #19413, #22812 ) ;
#22106 = DIRECTION ( 'NONE',  ( 0.000000000000000000, 0.000000000000000000, 1.000000000000000000 ) ) ;
#22107 = AXIS2_PLACEMENT_3D ( 'NONE', #9743, #446, #312 ) ;
#22108 = ORIENTED_EDGE ( 'NONE', *, *, #12374, .T. ) ;
#22109 = CARTESIAN_POINT ( 'NONE',  ( -124.2796999450276587, 81.25594874576239590, 30.00000000000641620 ) ) ;
#22110 = ORIENTED_EDGE ( 'NONE', *, *, #18284, .T. ) ;
#22111 = CARTESIAN_POINT ( 'NONE',  ( -282.2000000000012960, -74.99999999999899103, -90.00000000000000000 ) ) ;
#22112 = CARTESIAN_POINT ( 'NONE',  ( -280.0000000000000000, 270.0000000000000000, -144.9999999999999716 ) ) ;
#22113 = CONTEXT_DEPENDENT_SHAPE_REPRESENTATION ( #23442, #808 ) ;
#22114 = ORIENTED_EDGE ( 'NONE', *, *, #1941, .T. ) ;
#22115 = CARTESIAN_POINT ( 'NONE',  ( 125.6594390352178152, -1090.745324718712254, 28.47118012353589478 ) ) ;
#22116 = VERTEX_POINT ( 'NONE', #5051 ) ;
#22117 = CARTESIAN_POINT ( 'NONE',  ( -280.0627246250094800, 273.0000000000000000, 145.3431883596743148 ) ) ;
#22118 = CARTESIAN_POINT ( 'NONE',  ( 133.1749347183805696, 79.30613235829001439, 27.57867027829823670 ) ) ;
#22119 = CARTESIAN_POINT ( 'NONE',  ( 4.000000000001088907, 1.658577278524410170, -3.531553309554541720 ) ) ;
#22120 = EDGE_CURVE ( 'NONE', #5795, #22646, #20340, .T. ) ;
#22121 = PRODUCT_DEFINITION_SHAPE ( 'NONE', 'NONE',  #6213 ) ;
#22122 = AXIS2_PLACEMENT_3D ( 'NONE', #14442, #5245, #1721 ) ;
#22123 = FACE_BOUND ( 'NONE', #8348, .T. ) ;
#22124 = PLANE ( 'NONE',  #18468 ) ;
#22125 = DIRECTION ( 'NONE',  ( 1.000000000000000000, 0.000000000000000000, 0.000000000000000000 ) ) ;
#22126 = EDGE_CURVE ( 'NONE', #4603, #21251, #7231, .T. ) ;
#22127 = ADVANCED_FACE ( 'NONE', ( #15920 ), #6728, .F. ) ;
#22128 = EDGE_LOOP ( 'NONE', ( #16872, #17980, #15540, #1109, #1573 ) ) ;
#22129 = CARTESIAN_POINT ( 'NONE',  ( -7.327471962526033167E-12, -704.4690652294824531, 0.000000000000000000 ) ) ;
#22130 = CARTESIAN_POINT ( 'NONE',  ( -7.500000000000001776, 0.000000000000000000, 0.000000000000000000 ) ) ;
#22131 = DIRECTION ( 'NONE',  ( 1.110223024625157172E-14, 0.000000000000000000, -1.000000000000000000 ) ) ;
#22132 = ORIENTED_EDGE ( 'NONE', *, *, #9009, .F. ) ;
#22133 = EDGE_CURVE ( 'NONE', #7849, #13071, #17155, .T. ) ;
#22134 = CARTESIAN_POINT ( 'NONE',  ( -146.0000000000001137, -784.4690652294805204, 27.94500000000641649 ) ) ;
#22135 = DIRECTION ( 'NONE',  ( 0.000000000000000000, 0.000000000000000000, -1.000000000000000000 ) ) ;
#22136 = EDGE_CURVE ( 'NONE', #23462, #7849, #309, .T. ) ;
#22137 = CARTESIAN_POINT ( 'NONE',  ( 7.499999999999999112, 2.575910028905302074, -0.3641256808890108720 ) ) ;
#22138 = AXIS2_PLACEMENT_3D ( 'NONE', #15177, #5977, #13386 ) ;
#22139 = VECTOR ( 'NONE', #6447, 1000.000000000000000 ) ;
#22140 = DIRECTION ( 'NONE',  ( 0.000000000000000000, -0.5000000000000009992, -0.8660254037844380415 ) ) ;
#22141 = CARTESIAN_POINT ( 'NONE',  ( 281.2439791848364052, 269.1488036478620529, -150.0335297745770902 ) ) ;
#22142 = ORIENTED_EDGE ( 'NONE', *, *, #4638, .F. ) ;
#22143 = VECTOR ( 'NONE', #12139, 1000.000000000000000 ) ;
#22144 = CARTESIAN_POINT ( 'NONE',  ( 126.3653543294818178, 77.28387428943173632, -27.94499999999358053 ) ) ;
#22145 = ORIENTED_EDGE ( 'NONE', *, *, #2812, .T. ) ;
#22146 = AXIS2_PLACEMENT_3D ( 'NONE', #19082, #855, #180 ) ;
#22147 = DIRECTION ( 'NONE',  ( 1.110223024625156383E-14, -1.000000000000000000, 0.000000000000000000 ) ) ;
#22148 = FILL_AREA_STYLE ('',( #5738 ) ) ;
#22149 = DIRECTION ( 'NONE',  ( -0.000000000000000000, -0.000000000000000000, 1.000000000000000000 ) ) ;
#22150 = ORIENTED_EDGE ( 'NONE', *, *, #1046, .T. ) ;
#22151 = DIRECTION ( 'NONE',  ( -1.000000000000000000, -0.000000000000000000, -0.000000000000000000 ) ) ;
#22152 = CARTESIAN_POINT ( 'NONE',  ( 281.4928932188134354, 267.8000000000000114, -150.1999999999999318 ) ) ;
#22153 = CARTESIAN_POINT ( 'NONE',  ( -146.0000000000005116, -494.4690652294800657, -29.99999999999356604 ) ) ;
#22154 = CARTESIAN_POINT ( 'NONE',  ( 126.7787238282401319, 77.44864885511553609, -27.49999999999356248 ) ) ;
#22155 = LINE ( 'NONE', #9141, #7666 ) ;
#22156 = DIRECTION ( 'NONE',  ( 0.000000000000000000, 0.000000000000000000, 1.000000000000000000 ) ) ;
#22157 = CARTESIAN_POINT ( 'NONE',  ( -288.2000000000008981, 30.00000000000101963, -102.3500000000000369 ) ) ;
#22158 = ORIENTED_EDGE ( 'NONE', *, *, #3849, .T. ) ;
#22159 = VERTEX_POINT ( 'NONE', #22152 ) ;
#22160 = DIRECTION ( 'NONE',  ( 3.495664435217746987E-15, 1.000000000000000000, -0.000000000000000000 ) ) ;
#22161 = DIRECTION ( 'NONE',  ( -1.350636282998972974E-14, 0.000000000000000000, -1.000000000000000000 ) ) ;
#22162 = ORIENTED_EDGE ( 'NONE', *, *, #1212, .T. ) ;
#22163 = CIRCLE ( 'NONE', #11037, 2.055000000000000160 ) ;
#22164 = VECTOR ( 'NONE', #23775, 1000.000000000000000 ) ;
#22165 = FACE_OUTER_BOUND ( 'NONE', #6898, .T. ) ;
#22166 = CARTESIAN_POINT ( 'NONE',  ( 5.112021521198788498, -5.708827036477115868, -7.069802615102037890 ) ) ;
#22167 = EDGE_CURVE ( 'NONE', #16172, #11184, #4555, .T. ) ;
#22168 = EDGE_CURVE ( 'NONE', #22922, #8689, #170, .T. ) ;
#22169 = EDGE_CURVE ( 'NONE', #13199, #17672, #19991, .T. ) ;
#22170 = CARTESIAN_POINT ( 'NONE',  ( 280.2905802150185082, 269.9999999999999432, -145.1255313583546922 ) ) ;
#22171 = ORIENTED_EDGE ( 'NONE', *, *, #12155, .F. ) ;
#22172 = AXIS2_PLACEMENT_3D ( 'NONE', #13201, #22314, #2267 ) ;
#22173 = CARTESIAN_POINT ( 'NONE',  ( -5.384454397937118664, 6.594054843588581554E-16, -4.484454397937119197 ) ) ;
#22174 = DIRECTION ( 'NONE',  ( 3.469446951953614682E-16, -1.000000000000000000, 3.483493295888648978E-15 ) ) ;
#22175 = CARTESIAN_POINT ( 'NONE',  ( -7.996668423981801332, -6.145467199749147902, 200.0000120000000265 ) ) ;
#22176 = VERTEX_POINT ( 'NONE', #22042 ) ;
#22177 = CARTESIAN_POINT ( 'NONE',  ( -100.0000000000001137, -129.2000000000000455, 152.4000000000014268 ) ) ;
#22178 = CARTESIAN_POINT ( 'NONE',  ( -136.5854636148302461, -1073.276359373527839, 28.11170275877352509 ) ) ;
#22179 = DIRECTION ( 'NONE',  ( -1.000000000000000000, 0.000000000000000000, 0.000000000000000000 ) ) ;
#22180 = ORIENTED_EDGE ( 'NONE', *, *, #1733, .T. ) ;
#22181 = CARTESIAN_POINT ( 'NONE',  ( 280.6807971656550080, 272.9999999999999432, -145.1244294735508902 ) ) ;
#22182 = APPLICATION_PROTOCOL_DEFINITION ( 'draft international standard', 'automotive_design', 1998, #20316 ) ;
#22183 = AXIS2_PLACEMENT_3D ( 'NONE', #10039, #15699, #17392 ) ;
#22184 = CARTESIAN_POINT ( 'NONE',  ( -127.2680799365778199, 88.47518962644144835, -32.24959887471652564 ) ) ;
#22185 = CARTESIAN_POINT ( 'NONE',  ( -7.779103221381273414, 4.168986698926021361, -7.929128246061903695 ) ) ;
#22186 = FACE_OUTER_BOUND ( 'NONE', #21353, .T. ) ;
#22187 = ORIENTED_EDGE ( 'NONE', *, *, #9220, .F. ) ;
#22188 = ORIENTED_EDGE ( 'NONE', *, *, #21692, .F. ) ;
#22189 = CARTESIAN_POINT ( 'NONE',  ( -15.24974479720505904, -19.87769063953886572, 145.0000119999999697 ) ) ;
#22190 = AXIS2_PLACEMENT_3D ( 'NONE', #16844, #302, #20572 ) ;
#22191 = AXIS2_PLACEMENT_3D ( 'NONE', #6888, #17632, #5089 ) ;
#22192 = EDGE_CURVE ( 'NONE', #20235, #3630, #8420, .T. ) ;
#22193 = UNCERTAINTY_MEASURE_WITH_UNIT (LENGTH_MEASURE( 1.000000000000000082E-05 ), #4714, 'distance_accuracy_value', 'NONE');
#22194 = EDGE_LOOP ( 'NONE', ( #7145, #21460, #12216, #16634 ) ) ;
#22195 = AXIS2_PLACEMENT_3D ( 'NONE', #18262, #3529, #22236 ) ;
#22196 = DIRECTION ( 'NONE',  ( 0.000000000000000000, 1.000000000000000000, 0.000000000000000000 ) ) ;
#22197 = EDGE_CURVE ( 'NONE', #10116, #5111, #20113, .T. ) ;
#22198 = DIRECTION ( 'NONE',  ( 1.350636282998972974E-14, 0.000000000000000000, -1.000000000000000000 ) ) ;
#22199 = ORIENTED_EDGE ( 'NONE', *, *, #12148, .T. ) ;
#22200 =( REPRESENTATION_RELATIONSHIP ('NONE','NONE', #10127, #6236 ) REPRESENTATION_RELATIONSHIP_WITH_TRANSFORMATION ( #5005 )SHAPE_REPRESENTATION_RELATIONSHIP( ) );
#22201 = CARTESIAN_POINT ( 'NONE',  ( -44.99999999999997868, -52.79999999999939320, 137.3500000000001648 ) ) ;
#22202 = ORIENTED_EDGE ( 'NONE', *, *, #13454, .T. ) ;
#22203 = AXIS2_PLACEMENT_3D ( 'NONE', #3164, #5110, #14774 ) ;
#22204 = CARTESIAN_POINT ( 'NONE',  ( 153.5653415408403646, -1122.352966361445169, 30.00000000000675726 ) ) ;
#22205 = DIRECTION ( 'NONE',  ( -0.000000000000000000, -0.000000000000000000, 1.000000000000000000 ) ) ;
#22206 = ORIENTED_EDGE ( 'NONE', *, *, #3662, .T. ) ;
#22207 = DIRECTION ( 'NONE',  ( 0.000000000000000000, 0.000000000000000000, -1.000000000000000000 ) ) ;
#22208 = DIRECTION ( 'NONE',  ( 1.000000000000000000, 0.000000000000000000, 0.000000000000000000 ) ) ;
#22209 = CARTESIAN_POINT ( 'NONE',  ( -281.4928932188134354, -127.0000000000000568, -152.4000000000012847 ) ) ;
#22210 = CARTESIAN_POINT ( 'NONE',  ( -282.2000000000014666, -127.0000000000000568, -146.4928932188134070 ) ) ;
#22211 = CARTESIAN_POINT ( 'NONE',  ( 125.7666110541939588, -1090.596734011949366, -28.73951976925631513 ) ) ;
#22212 = CARTESIAN_POINT ( 'NONE',  ( 285.2000000000013529, -127.0000000000000568, -146.4928932188134070 ) ) ;
#22213 = VERTEX_POINT ( 'NONE', #5748 ) ;
#22214 = FACE_BOUND ( 'NONE', #8232, .T. ) ;
#22215 = LINE ( 'NONE', #3874, #2044 ) ;
#22216 = ADVANCED_FACE ( 'NONE', ( #5502 ), #11222, .F. ) ;
#22218 = ORIENTED_EDGE ( 'NONE', *, *, #10602, .T. ) ;
#22217 = ORIENTED_EDGE ( 'NONE', *, *, #21627, .F. ) ;
#22219 = DIRECTION ( 'NONE',  ( 0.000000000000000000, 0.000000000000000000, 1.000000000000000000 ) ) ;
#22220 = LINE ( 'NONE', #7499, #397 ) ;
#22221 = AXIS2_PLACEMENT_3D ( 'NONE', #12130, #6532, #12025 ) ;
#22222 = FACE_OUTER_BOUND ( 'NONE', #8804, .T. ) ;
#22223 = DIRECTION ( 'NONE',  ( 0.000000000000000000, 0.000000000000000000, -1.000000000000000000 ) ) ;
#22224 = ORIENTED_EDGE ( 'NONE', *, *, #7106, .F. ) ;
#22225 = CARTESIAN_POINT ( 'NONE',  ( -134.5482912860055080, -1076.952955187287444, 30.16873261443285870 ) ) ;
#22226 = ORIENTED_EDGE ( 'NONE', *, *, #585, .F. ) ;
#22227 = EDGE_CURVE ( 'NONE', #8057, #4317, #8024, .T. ) ;
#22228 = CARTESIAN_POINT ( 'NONE',  ( 155.0000000000000568, -1000.000000000000000, 90.00000000000000000 ) ) ;
#22229 = ORIENTED_EDGE ( 'NONE', *, *, #9906, .T. ) ;
#22230 = DIRECTION ( 'NONE',  ( 0.000000000000000000, 0.000000000000000000, 1.000000000000000000 ) ) ;
#22231 = CARTESIAN_POINT ( 'NONE',  ( -44.99999999999995026, -59.79999999999967741, 107.6500000000002331 ) ) ;
#22232 = ADVANCED_FACE ( 'NONE', ( #3917 ), #23435, .F. ) ;
#22233 = AXIS2_PLACEMENT_3D ( 'NONE', #5796, #18570, #21966 ) ;
#22234 = CONTEXT_DEPENDENT_SHAPE_REPRESENTATION ( #1998, #8331 ) ;
#22235 = ORIENTED_EDGE ( 'NONE', *, *, #8843, .F. ) ;
#22236 = DIRECTION ( 'NONE',  ( 0.000000000000000000, -2.618450529776313049E-15, -1.000000000000000000 ) ) ;
#22237 = ORIENTED_EDGE ( 'NONE', *, *, #703, .T. ) ;
#22238 = CIRCLE ( 'NONE', #23017, 35.00000000000000711 ) ;
#22239 = CARTESIAN_POINT ( 'NONE',  ( -280.7774350431396897, 271.3570580646226063, 148.7968359015656574 ) ) ;
#22240 = CARTESIAN_POINT ( 'NONE',  ( 5.200000000000002842, 3.061616997868383634E-16, -2.500000000000000444 ) ) ;
#22241 = PLANE ( 'NONE',  #23456 ) ;
#22242 = CARTESIAN_POINT ( 'NONE',  ( 10.00000000000000000, 8.000000000000000000, 0.000000000000000000 ) ) ;
#22243 = CARTESIAN_POINT ( 'NONE',  ( -280.2905802150187355, 270.0000000000000000, 145.1255313583548059 ) ) ;
#22244 = EDGE_LOOP ( 'NONE', ( #653, #5093, #14418, #14165, #15526 ) ) ;
#22245 = DIRECTION ( 'NONE',  ( 1.000000000000000000, 0.000000000000000000, 0.000000000000000000 ) ) ;
#22246 = DIRECTION ( 'NONE',  ( 1.000000000000000000, 0.000000000000000000, 0.000000000000000000 ) ) ;
#22247 = DIRECTION ( 'NONE',  ( -2.775557561562891351E-17, 1.000000000000000000, -2.081668171172166936E-15 ) ) ;
#22248 = AXIS2_PLACEMENT_3D ( 'NONE', #12691, #3336, #3806 ) ;
#22249 = CARTESIAN_POINT ( 'NONE',  ( 282.1999999999999318, 267.7999999999999545, 146.4928932188134922 ) ) ;
#22250 = EDGE_CURVE ( 'NONE', #1506, #23662, #8526, .T. ) ;
#22251 = CARTESIAN_POINT ( 'NONE',  ( 145.0000000000000284, 1.518794382396763073E-12, -90.00000000000000000 ) ) ;
#22252 = EDGE_CURVE ( 'NONE', #5073, #16206, #6339, .T. ) ;
#22253 = VECTOR ( 'NONE', #19463, 1000.000000000000000 ) ;
#22254 = VECTOR ( 'NONE', #1558, 1000.000000000000000 ) ;
#22255 = AXIS2_PLACEMENT_3D ( 'NONE', #8862, #21999, #1238 ) ;
#22256 = ADVANCED_BREP_SHAPE_REPRESENTATION ( '', ( #12608, #11210 ), #7665 ) ;
#22257 = CARTESIAN_POINT ( 'NONE',  ( -24.99999999999998224, -1000.000000000000000, 145.0000059999999280 ) ) ;
#22258 = LINE ( 'NONE', #16726, #21962 ) ;
#22259 = EDGE_CURVE ( 'NONE', #3693, #10547, #21897, .T. ) ;
#22260 = CONTEXT_DEPENDENT_SHAPE_REPRESENTATION ( #10501, #6603 ) ;
#22261 = VERTEX_POINT ( 'NONE', #8279 ) ;
#22262 = CARTESIAN_POINT ( 'NONE',  ( -24.20041621714723945, -993.5179357872719947, 145.0000119999999697 ) ) ;
#22263 = ADVANCED_FACE ( 'NONE', ( #4526 ), #5980, .T. ) ;
#22264 = ORIENTED_EDGE ( 'NONE', *, *, #23033, .T. ) ;
#22265 = DIRECTION ( 'NONE',  ( -1.000000000000000000, 0.000000000000000000, 0.000000000000000000 ) ) ;
#22266 = LINE ( 'NONE', #17981, #14495 ) ;
#22267 = LINE ( 'NONE', #7668, #20208 ) ;
#22268 = VERTEX_POINT ( 'NONE', #2471 ) ;
#22269 = VECTOR ( 'NONE', #11067, 1000.000000000000000 ) ;
#22270 = LINE ( 'NONE', #553, #4984 ) ;
#22271 = ADVANCED_FACE ( 'NONE', ( #13270 ), #19129, .T. ) ;
#22272 = CARTESIAN_POINT ( 'NONE',  ( 5.000000000000000000, 4.685197434473814759, -5.637851296924623057E-15 ) ) ;
#22273 = CARTESIAN_POINT ( 'NONE',  ( -24.99999999999995381, -52.79999999999975557, 35.00000000000017764 ) ) ;
#22274 = FACE_OUTER_BOUND ( 'NONE', #16450, .T. ) ;
#22275 = CARTESIAN_POINT ( 'NONE',  ( 0.000000000000000000, 0.000000000000000000, 0.000000000000000000 ) ) ;
#22276 = EDGE_CURVE ( 'NONE', #12669, #21242, #18804, .T. ) ;
#22277 = CARTESIAN_POINT ( 'NONE',  ( 0.000000000000000000, 0.000000000000000000, -90.00000000000000000 ) ) ;
#22278 = AXIS2_PLACEMENT_3D ( 'NONE', #1374, #21199, #8761 ) ;
#22279 = CARTESIAN_POINT ( 'NONE',  ( -7.500000000000000000, -1.572902445675612659, -7.069816568113127531 ) ) ;
#22280 = AXIS2_PLACEMENT_3D ( 'NONE', #6118, #13403, #7688 ) ;
#22281 = ORIENTED_EDGE ( 'NONE', *, *, #15119, .F. ) ;
#22282 = DIRECTION ( 'NONE',  ( -1.000000000000000000, -0.000000000000000000, -0.000000000000000000 ) ) ;
#22283 = DIRECTION ( 'NONE',  ( 1.000000000000000000, 0.000000000000000000, 0.000000000000000000 ) ) ;
#22284 = ORIENTED_EDGE ( 'NONE', *, *, #19331, .F. ) ;
#22285 = LINE ( 'NONE', #7092, #4588 ) ;
#22286 = CARTESIAN_POINT ( 'NONE',  ( -137.9031948627974486, 44.80746418436699940, -90.00000000000000000 ) ) ;
#22287 = CARTESIAN_POINT ( 'NONE',  ( 282.1999999999999886, 267.9452901038201844, -146.4301275412296945 ) ) ;
#22288 = VERTEX_POINT ( 'NONE', #794 ) ;
#22289 = ADVANCED_FACE ( 'NONE', ( #2588 ), #20702, .F. ) ;
#22290 = VECTOR ( 'NONE', #7379, 1000.000000000000000 ) ;
#22291 = CARTESIAN_POINT ( 'NONE',  ( -3.349226789952655547, -2.685125164760744809, -0.2236248678334863682 ) ) ;
#22292 = FACE_OUTER_BOUND ( 'NONE', #12698, .T. ) ;
#22293 = EDGE_CURVE ( 'NONE', #22490, #23365, #6102, .T. ) ;
#22294 = TOROIDAL_SURFACE ( 'NONE', #6109, 10.12668159690567649, 0.7733184030943209830 ) ;
#22295 = CARTESIAN_POINT ( 'NONE',  ( 126.3653543294811499, 77.28387428943223370, 27.94500000000640227 ) ) ;
#22296 = EDGE_LOOP ( 'NONE', ( #10451, #6014, #22560, #772, #18778, #12007, #3517, #18657, #1402, #11856, #4287, #22973, #12215, #1251, #5586, #22040, #14962, #2947, #2081, #8138, #17216, #22467, #3524, #19702, #450, #18218, #6173, #15367, #8627, #8252, #10329, #89, #13930, #7490, #1486, #18320, #16943, #17292, #13268, #16391, #14275, #4539, #12707, #9103, #8317, #12993, #19017, #11084, #21830 ) ) ;
#22297 = LINE ( 'NONE', #20490, #22552 ) ;
#22298 = CARTESIAN_POINT ( 'NONE',  ( 7.703011046602857601E-15, -132.2000000000000455, 0.000000000000000000 ) ) ;
#22299 = ADVANCED_FACE ( 'NONE', ( #21070, #11447, #16988, #668, #444 ), #7795, .T. ) ;
#22300 = AXIS2_PLACEMENT_3D ( 'NONE', #1400, #23509, #1632 ) ;
#22301 = CARTESIAN_POINT ( 'NONE',  ( 5.200000000000002842, 0.000000000000000000, 0.000000000000000000 ) ) ;
#22302 = ORIENTED_EDGE ( 'NONE', *, *, #22098, .F. ) ;
#22303 = CYLINDRICAL_SURFACE ( 'NONE', #3062, 35.00000000000000711 ) ;
#22304 = APPLICATION_PROTOCOL_DEFINITION ( 'draft international standard', 'automotive_design', 1998, #1505 ) ;
#22305 = CARTESIAN_POINT ( 'NONE',  ( -155.0000000000000284, -494.4690652294806341, 27.50000000000647660 ) ) ;
#22306 = EDGE_CURVE ( 'NONE', #1398, #17675, #15427, .T. ) ;
#22307 = ADVANCED_FACE ( 'NONE', ( #19254 ), #18894, .F. ) ;
#22308 = CARTESIAN_POINT ( 'NONE',  ( 2.500000000000000000, -2.357898499370432610, 3.252606517456513302E-15 ) ) ;
#22309 = CARTESIAN_POINT ( 'NONE',  ( 5.000000000000004441, 0.000000000000000000, 0.000000000000000000 ) ) ;
#22310 = EDGE_LOOP ( 'NONE', ( #15810, #887, #20354, #23147 ) ) ;
#22311 = ORIENTED_EDGE ( 'NONE', *, *, #22088, .T. ) ;
#22312 = AXIS2_PLACEMENT_3D ( 'NONE', #18775, #6351, #20591 ) ;
#22313 = DIRECTION ( 'NONE',  ( -0.000000000000000000, -0.000000000000000000, 1.000000000000000000 ) ) ;
#22314 = DIRECTION ( 'NONE',  ( 1.000000000000000000, -0.000000000000000000, 6.982962677686266711E-15 ) ) ;
#22315 = AXIS2_PLACEMENT_3D ( 'NONE', #19161, #10018, #1047 ) ;
#22316 = VECTOR ( 'NONE', #7400, 1000.000000000000000 ) ;
#22317 = CIRCLE ( 'NONE', #13874, 2.649999999999999467 ) ;
#22318 = UNCERTAINTY_MEASURE_WITH_UNIT (LENGTH_MEASURE( 1.000000000000000082E-05 ), #3238, 'distance_accuracy_value', 'NONE');
#22319 = ORIENTED_EDGE ( 'NONE', *, *, #267, .F. ) ;
#22320 = CARTESIAN_POINT ( 'NONE',  ( -194.7500000000000000, -494.4690652294800657, 32.50000000000675726 ) ) ;
#22321 = DIRECTION ( 'NONE',  ( 0.5877852522924719159, 0.8090169943749482284, 0.000000000000000000 ) ) ;
#22322 = VERTEX_POINT ( 'NONE', #4032 ) ;
#22323 = CARTESIAN_POINT ( 'NONE',  ( -45.24999999999994316, 100.0000000000000000, -147.2000000000005571 ) ) ;
#22324 = ORIENTED_EDGE ( 'NONE', *, *, #11312, .T. ) ;
#22325 = AXIS2_PLACEMENT_3D ( 'NONE', #20549, #22372, #9711 ) ;
#22326 = AXIS2_PLACEMENT_3D ( 'NONE', #17913, #10934, #14198 ) ;
#22328 = AXIS2_PLACEMENT_3D ( 'NONE', #7640, #19101, #9954 ) ;
#22327 = MECHANICAL_DESIGN_GEOMETRIC_PRESENTATION_REPRESENTATION (  '', ( #15789 ), #7690 ) ;
#22330 =( NAMED_UNIT ( * ) SI_UNIT ( $, .STERADIAN. ) SOLID_ANGLE_UNIT ( ) );
#22329 = CIRCLE ( 'NONE', #1883, 35.00000000000000711 ) ;
#22331 = CIRCLE ( 'NONE', #21958, 145.0000000000000284 ) ;
#22333 = AXIS2_PLACEMENT_3D ( 'NONE', #14076, #22817, #15488 ) ;
#22332 = CYLINDRICAL_SURFACE ( 'NONE', #13286, 5.249999999999973355 ) ;
#22334 = ORIENTED_EDGE ( 'NONE', *, *, #22192, .F. ) ;
#22335 = CARTESIAN_POINT ( 'NONE',  ( -5.274401269815139237, -6.074457022762090652, -7.633824513837113912 ) ) ;
#22336 = VECTOR ( 'NONE', #15642, 1000.000000000000000 ) ;
#22337 = CIRCLE ( 'NONE', #7673, 2.499999999999998668 ) ;
#22338 = DIRECTION ( 'NONE',  ( -1.000000000000000000, 0.000000000000000000, -0.000000000000000000 ) ) ;
#22339 = EDGE_CURVE ( 'NONE', #19885, #2929, #21136, .T. ) ;
#22340 = DIRECTION ( 'NONE',  ( 0.000000000000000000, 0.000000000000000000, 1.000000000000000000 ) ) ;
#22341 = EDGE_CURVE ( 'NONE', #4703, #19969, #21992, .T. ) ;
#22342 = CYLINDRICAL_SURFACE ( 'NONE', #5324, 5.199999999999982414 ) ;
#22343 = DIRECTION ( 'NONE',  ( 0.9289202219288174023, 0.3702799228849934510, 6.982962677686266711E-15 ) ) ;
#22344 = EDGE_CURVE ( 'NONE', #12593, #2692, #17094, .T. ) ;
#22345 = CARTESIAN_POINT ( 'NONE',  ( -45.24999999999994316, 100.0000000000000000, 150.2000000000009550 ) ) ;
#22346 = ORIENTED_EDGE ( 'NONE', *, *, #13032, .F. ) ;
#22347 = CARTESIAN_POINT ( 'NONE',  ( 0.000000000000000000, 0.000000000000000000, -138.9999999999999716 ) ) ;
#22348 = CARTESIAN_POINT ( 'NONE',  ( -20.63749999999999574, 0.000000000000000000, 0.000000000000000000 ) ) ;
#22350 = VERTEX_POINT ( 'NONE', #18047 ) ;
#22349 = ORIENTED_EDGE ( 'NONE', *, *, #12694, .F. ) ;
#22352 = CIRCLE ( 'NONE', #12002, 2.649999999999971934 ) ;
#22351 = AXIS2_PLACEMENT_3D ( 'NONE', #20558, #4012, #18736 ) ;
#22353 = CARTESIAN_POINT ( 'NONE',  ( -146.0000000000005400, -204.4690652294800657, -32.05499999999356930 ) ) ;
#22354 = CARTESIAN_POINT ( 'NONE',  ( 281.4928932188134354, 267.8000000000000114, -150.1999999999999318 ) ) ;
#22355 = COLOUR_RGB ( '',0.8941176470588234615, 0.8941176470588234615, 0.8941176470588234615 ) ;
#22356 = VECTOR ( 'NONE', #13971, 1000.000000000000000 ) ;
#22357 = TOROIDAL_SURFACE ( 'NONE', #7696, 2.700000000000000622, 0.2000000000000000111 ) ;
#22358 = ORIENTED_EDGE ( 'NONE', *, *, #15516, .F. ) ;
#22359 = DIRECTION ( 'NONE',  ( -1.000000000000000000, 0.000000000000000000, 0.000000000000000000 ) ) ;
#22360 = ORIENTED_EDGE ( 'NONE', *, *, #14684, .F. ) ;
#22361 = CARTESIAN_POINT ( 'NONE',  ( 285.0327955282141374, 269.1518577254344677, -146.2434055557878025 ) ) ;
#22362 = CIRCLE ( 'NONE', #12790, 7.499999999999996447 ) ;
#22363 = EDGE_LOOP ( 'NONE', ( #12068, #1793 ) ) ;
#22364 = LINE ( 'NONE', #11408, #15804 ) ;
#22365 = FACE_OUTER_BOUND ( 'NONE', #23235, .T. ) ;
#22366 = ORIENTED_EDGE ( 'NONE', *, *, #14261, .T. ) ;
#22367 = CARTESIAN_POINT ( 'NONE',  ( 80.00000000000001421, -59.79999999999998295, 5.199999999999996625 ) ) ;
#22368 = AXIS2_PLACEMENT_3D ( 'NONE', #9337, #23682, #1818 ) ;
#22369 = ORIENTED_EDGE ( 'NONE', *, *, #19903, .T. ) ;
#22370 = CARTESIAN_POINT ( 'NONE',  ( -128.0869692137160598, 87.28547799715779831, 32.48437713430730156 ) ) ;
#22371 = CIRCLE ( 'NONE', #22312, 145.0000000000000284 ) ;
#22372 = DIRECTION ( 'NONE',  ( 0.000000000000000000, 0.000000000000000000, 1.000000000000000000 ) ) ;
#22373 = AXIS2_PLACEMENT_3D ( 'NONE', #1208, #17618, #17404 ) ;
#22374 = AXIS2_PLACEMENT_3D ( 'NONE', #14689, #16361, #21896 ) ;
#22375 = EDGE_CURVE ( 'NONE', #20294, #11363, #16894, .T. ) ;
#22376 = FACE_OUTER_BOUND ( 'NONE', #14050, .T. ) ;
#22377 = CARTESIAN_POINT ( 'NONE',  ( 119.6158142514527327, -1087.367367941136308, 30.00000000000641620 ) ) ;
#22378 = VERTEX_POINT ( 'NONE', #3178 ) ;
#22379 = CARTESIAN_POINT ( 'NONE',  ( -280.4976310729378497, 272.3436892194421262, -147.6188186979286741 ) ) ;
#22380 =( NAMED_UNIT ( * ) SI_UNIT ( $, .STERADIAN. ) SOLID_ANGLE_UNIT ( ) );
#22381 = ORIENTED_EDGE ( 'NONE', *, *, #15203, .F. ) ;
#22382 = DIRECTION ( 'NONE',  ( 6.982962677686266711E-15, 0.000000000000000000, -1.000000000000000000 ) ) ;
#22383 = DIRECTION ( 'NONE',  ( 0.000000000000000000, 0.000000000000000000, -1.000000000000000000 ) ) ;
#22384 = CARTESIAN_POINT ( 'NONE',  ( 131.6538433078038963, 81.80629369879927992, -28.88328940716461801 ) ) ;
#22385 = CARTESIAN_POINT ( 'NONE',  ( 285.1999999999999318, 267.7999999999999545, 146.4928932188134922 ) ) ;
#22386 = LINE ( 'NONE', #9725, #2549 ) ;
#22387 = DIRECTION ( 'NONE',  ( -0.7071067811865310304, 8.659560562355135004E-17, -0.7071067811865641151 ) ) ;
#22388 = B_SPLINE_CURVE_WITH_KNOTS ( 'NONE', 3,
 ( #18583, #6810, #5812, #25, #14754, #9546, #18475, #5009, #13216, #20516, #5559, #23464, #7376, #3966, #16116, #8751, #21537, #6932, #16907, #2156, #11382, #14203, #14334, #12422, #3174, #10581, #21662, #5120 ),
 .UNSPECIFIED., .F., .F.,
 ( 4, 2, 2, 2, 2, 2, 2, 2, 2, 2, 2, 2, 2, 4 ),
 ( 0.007862850516742125873, 0.008354729399060669900, 0.008846608281379213928, 0.009830366046016345352, 0.01032224492833490673, 0.01081412381065346810, 0.01130600269297203121, 0.01179788157529059259, 0.01278163933992771707, 0.01327351822224628886, 0.01376539710456485890, 0.01425727598688343069, 0.01474915486920200074, 0.01573291263383913216 ),
 .UNSPECIFIED. ) ;
#22389 = CARTESIAN_POINT ( 'NONE',  ( 29.55500000000002458, 3.061616997868375746E-16, -2.500000000000000888 ) ) ;
#22390 = CARTESIAN_POINT ( 'NONE',  ( -7.499999999999999112, 0.000000000000000000, 100.0000000000000000 ) ) ;
#22391 = ORIENTED_EDGE ( 'NONE', *, *, #14682, .F. ) ;
#22392 = FACE_OUTER_BOUND ( 'NONE', #2399, .T. ) ;
#22393 = ORIENTED_EDGE ( 'NONE', *, *, #2730, .F. ) ;
#22394 = CARTESIAN_POINT ( 'NONE',  ( 281.4928932188133786, 267.7999999999999545, 150.1999999999999886 ) ) ;
#22395 = CARTESIAN_POINT ( 'NONE',  ( 279.9999999999999432, 267.7999999999999545, 150.1999999999999886 ) ) ;
#22396 = CARTESIAN_POINT ( 'NONE',  ( -90.00000000000000000, -149.9999999999996874, 129.9038105676659711 ) ) ;
#22397 = ORIENTED_EDGE ( 'NONE', *, *, #3086, .T. ) ;
#22398 = DIRECTION ( 'NONE',  ( 0.000000000000000000, -0.000000000000000000, 1.000000000000000000 ) ) ;
#22399 = CARTESIAN_POINT ( 'NONE',  ( 124.4701338314433201, -1092.369831568443260, -32.49999999999351985 ) ) ;
#22400 = ADVANCED_FACE ( 'NONE', ( #23230 ), #21543, .T. ) ;
#22401 = CARTESIAN_POINT ( 'NONE',  ( -31.74999999999995737, 6.123233995736768255E-16, -5.000000000000001776 ) ) ;
#22402 = CARTESIAN_POINT ( 'NONE',  ( 2.344047193898588954, 3.265465875126468021, -5.031375706690542042E-16 ) ) ;
#22403 = FACE_OUTER_BOUND ( 'NONE', #11937, .T. ) ;
#22404 = EDGE_CURVE ( 'NONE', #679, #13773, #17642, .T. ) ;
#22405 = PLANE ( 'NONE',  #9222 ) ;
#22406 = EDGE_CURVE ( 'NONE', #4361, #12504, #1260, .T. ) ;
#22407 = CARTESIAN_POINT ( 'NONE',  ( -7.500000000000346390, -3.105855721450154316, -7.659356991636309786 ) ) ;
#22408 = ORIENTED_EDGE ( 'NONE', *, *, #14082, .F. ) ;
#22409 =( LENGTH_UNIT ( ) NAMED_UNIT ( * ) SI_UNIT ( .MILLI., .METRE. ) );
#22410 = DIRECTION ( 'NONE',  ( 0.000000000000000000, 1.000000000000000000, 1.177509268541832635E-16 ) ) ;
#22411 = CYLINDRICAL_SURFACE ( 'NONE', #8497, 5.249999999999942268 ) ;
#22412 = ADVANCED_FACE ( 'NONE', ( #4764 ), #1008, .F. ) ;
#22413 = ORIENTED_EDGE ( 'NONE', *, *, #4353, .F. ) ;
#22414 = ORIENTED_EDGE ( 'NONE', *, *, #14807, .T. ) ;
#22415 = DIRECTION ( 'NONE',  ( -1.000000000000000000, -2.775557561562891351E-17, 0.000000000000000000 ) ) ;
#22416 = FACE_OUTER_BOUND ( 'NONE', #22487, .T. ) ;
#22417 = CARTESIAN_POINT ( 'NONE',  ( 2.500000000000000000, -2.357898499370432166, 3.035766082959412415E-15 ) ) ;
#22418 = VERTEX_POINT ( 'NONE', #14208 ) ;
#22419 = CARTESIAN_POINT ( 'NONE',  ( 281.4928932188134354, -132.2000000000000455, -152.4000000000013131 ) ) ;
#22420 = CARTESIAN_POINT ( 'NONE',  ( 2.621086668468698644, 7.606368536631364030, -7.634085501268425666 ) ) ;
#22421 = DIRECTION ( 'NONE',  ( 0.000000000000000000, 0.000000000000000000, 1.000000000000000000 ) ) ;
#22422 = EDGE_LOOP ( 'NONE', ( #9717, #4547, #9544, #22397 ) ) ;
#22423 = CARTESIAN_POINT ( 'NONE',  ( 280.8082263737021549, 271.2379565153279373, 148.9159870726003874 ) ) ;
#22424 = DIRECTION ( 'NONE',  ( 0.000000000000000000, -0.4999999999999992228, 0.8660254037844390407 ) ) ;
#22425 = DIRECTION ( 'NONE',  ( 0.000000000000000000, 0.000000000000000000, 1.000000000000000000 ) ) ;
#22426 = VERTEX_POINT ( 'NONE', #8888 ) ;
#22427 = CARTESIAN_POINT ( 'NONE',  ( 280.5679143846942907, 269.9132285165672442, -145.2488155364688680 ) ) ;
#22428 = APPLICATION_PROTOCOL_DEFINITION ( 'draft international standard', 'automotive_design', 1998, #19235 ) ;
#22429 = DIRECTION ( 'NONE',  ( 0.000000000000000000, -1.000000000000000000, 0.000000000000000000 ) ) ;
#22430 = DIRECTION ( 'NONE',  ( 1.000000000000000000, 3.736327486719276364E-16, 1.067522139062650425E-16 ) ) ;
#22431 = CARTESIAN_POINT ( 'NONE',  ( 4.250000000000000000, 0.000000000000000000, -0.5251556536572846712 ) ) ;
#22432 = VERTEX_POINT ( 'NONE', #12427 ) ;
#22433 = ORIENTED_EDGE ( 'NONE', *, *, #20096, .F. ) ;
#22434 = CARTESIAN_POINT ( 'NONE',  ( -100.0000000000001137, -132.1999999999999602, -113.4834095219707848 ) ) ;
#22435 = CARTESIAN_POINT ( 'NONE',  ( 282.1999999999999318, 267.7999999999999545, -144.9999999999999716 ) ) ;
#22436 = EDGE_CURVE ( 'NONE', #16206, #15650, #15765, .T. ) ;
#22437 = EDGE_CURVE ( 'NONE', #19785, #16807, #10551, .T. ) ;
#22438 = VERTEX_POINT ( 'NONE', #6455 ) ;
#22439 = DIRECTION ( 'NONE',  ( 0.000000000000000000, 0.000000000000000000, 1.000000000000000000 ) ) ;
#22440 = EDGE_CURVE ( 'NONE', #20130, #23533, #1456, .T. ) ;
#22441 = DIRECTION ( 'NONE',  ( -1.000000000000000000, -0.000000000000000000, -0.000000000000000000 ) ) ;
#22442 = PRODUCT_RELATED_PRODUCT_CATEGORY ( 'part', '', ( #4766 ) ) ;
#22443 = VERTEX_POINT ( 'NONE', #21667 ) ;
#22445 = ADVANCED_FACE ( 'NONE', ( #17926 ), #14095, .F. ) ;
#22444 = DIRECTION ( 'NONE',  ( 1.000000000000000000, 0.000000000000000000, 0.000000000000000000 ) ) ;
#22446 = AXIS2_PLACEMENT_3D ( 'NONE', #15319, #4545, #11963 ) ;
#22447 = EDGE_LOOP ( 'NONE', ( #9134, #3234 ) ) ;
#22448 = LINE ( 'NONE', #604, #7501 ) ;
#22449 = CARTESIAN_POINT ( 'NONE',  ( 1.734723475976807094E-15, 4.618802153517012954, -0.4999999999999995559 ) ) ;
#22450 = ORIENTED_EDGE ( 'NONE', *, *, #6978, .F. ) ;
#22451 = ORIENTED_EDGE ( 'NONE', *, *, #9929, .T. ) ;
#22452 = CARTESIAN_POINT ( 'NONE',  ( 0.000000000000000000, 0.000000000000000000, 200.0000000000000000 ) ) ;
#22453 = DIRECTION ( 'NONE',  ( 0.000000000000000000, -2.618450529776313049E-15, -1.000000000000000000 ) ) ;
#22454 = CARTESIAN_POINT ( 'NONE',  ( 8.050072860899410543, -1023.725408969439172, -145.0000000000001137 ) ) ;
#22455 = DIRECTION ( 'NONE',  ( 0.000000000000000000, -1.000000000000000000, 0.000000000000000000 ) ) ;
#22456 = CARTESIAN_POINT ( 'NONE',  ( 2.500000000000000000, 1.178949249685218525, 2.041999999999999371 ) ) ;
#22457 = CYLINDRICAL_SURFACE ( 'NONE', #7029, 2.500000000000002220 ) ;
#22458 = DIRECTION ( 'NONE',  ( -1.000000000000000000, -2.775557561562891351E-17, 0.000000000000000000 ) ) ;
#22459 = ORIENTED_EDGE ( 'NONE', *, *, #21115, .F. ) ;
#22460 = DIRECTION ( 'NONE',  ( 0.4924295582441756136, -0.5074575156280946020, -0.7071067811865532349 ) ) ;
#22461 = LINE ( 'NONE', #8117, #3717 ) ;
#22462 = AXIS2_PLACEMENT_3D ( 'NONE', #7953, #20874, #6139 ) ;
#22464 = ORIENTED_EDGE ( 'NONE', *, *, #14638, .T. ) ;
#22463 = ORIENTED_EDGE ( 'NONE', *, *, #13677, .F. ) ;
#22465 = CARTESIAN_POINT ( 'NONE',  ( 287.4000000000013415, -129.2000000000000455, -146.4928932188134070 ) ) ;
#22466 = CARTESIAN_POINT ( 'NONE',  ( 280.8708543776411943, 270.9956429438695977, -149.1582675804704650 ) ) ;
#22467 = ORIENTED_EDGE ( 'NONE', *, *, #3883, .T. ) ;
#22468 = DIRECTION ( 'NONE',  ( 0.000000000000000000, -1.000000000000000000, 0.000000000000000000 ) ) ;
#22469 = EDGE_CURVE ( 'NONE', #11416, #10663, #2987, .T. ) ;
#22470 = EDGE_CURVE ( 'NONE', #286, #10923, #1829, .T. ) ;
#22471 = EDGE_LOOP ( 'NONE', ( #13967, #9541, #11201, #8914 ) ) ;
#22472 = EDGE_CURVE ( 'NONE', #13321, #10981, #23117, .T. ) ;
#22473 = DIRECTION ( 'NONE',  ( 1.000000000000000000, 0.000000000000000000, 0.000000000000000000 ) ) ;
#22474 = VERTEX_POINT ( 'NONE', #12178 ) ;
#22475 = DIRECTION ( 'NONE',  ( -0.000000000000000000, -0.000000000000000000, 1.000000000000000000 ) ) ;
#22476 = CYLINDRICAL_SURFACE ( 'NONE', #7291, 7.500000000000007105 ) ;
#22477 = ITEM_DEFINED_TRANSFORMATION ( 'NONE', 'NONE', #13559,  #11210 ) ;
#22478 = ORIENTED_EDGE ( 'NONE', *, *, #16790, .T. ) ;
#22479 = AXIS2_PLACEMENT_3D ( 'NONE', #9990, #15775, #21203 ) ;
#22480 =( REPRESENTATION_RELATIONSHIP ('NONE','NONE', #10127, #6508 ) REPRESENTATION_RELATIONSHIP_WITH_TRANSFORMATION ( #6689 )SHAPE_REPRESENTATION_RELATIONSHIP( ) );
#22481 = DIRECTION ( 'NONE',  ( 1.000000000000000000, 0.000000000000000000, 0.000000000000000000 ) ) ;
#22482 = ORIENTED_EDGE ( 'NONE', *, *, #4746, .F. ) ;
#22483 = CARTESIAN_POINT ( 'NONE',  ( 6.487740029697272703, -975.8006625472378346, -145.0000000000001137 ) ) ;
#22484 = CARTESIAN_POINT ( 'NONE',  ( -67.34999999999996589, -112.6666666666667140, 148.0000000000000000 ) ) ;
#22485 = CARTESIAN_POINT ( 'NONE',  ( 140.0355749532213281, -37.61698748598472264, -90.00000000000000000 ) ) ;
#22486 = CARTESIAN_POINT ( 'NONE',  ( -77.72886158240878274, 117.3074641843673049, -90.00000000000000000 ) ) ;
#22487 = EDGE_LOOP ( 'NONE', ( #21470, #19895, #15499, #20547 ) ) ;
#22488 = CARTESIAN_POINT ( 'NONE',  ( -280.8708543776411943, 271.0140793454687582, -149.1822575857424624 ) ) ;
#22489 = CIRCLE ( 'NONE', #17114, 35.00000000000000000 ) ;
#22490 = VERTEX_POINT ( 'NONE', #19851 ) ;
#22491 = CARTESIAN_POINT ( 'NONE',  ( -7.327471962526033167E-12, -1284.469065229482339, 0.000000000000000000 ) ) ;
#22492 = CARTESIAN_POINT ( 'NONE',  ( 10.40000000000000036, 0.000000000000000000, 0.000000000000000000 ) ) ;
#22493 = CARTESIAN_POINT ( 'NONE',  ( -281.4928932188134354, -132.2000000000000455, -177.2000000000013529 ) ) ;
#22494 = CARTESIAN_POINT ( 'NONE',  ( 285.1999999999999318, 268.4807971656551331, 146.3684637452625168 ) ) ;
#22495 = CARTESIAN_POINT ( 'NONE',  ( 45.00000000000004974, -59.79999999999964899, 105.0000000000002274 ) ) ;
#22496 = ORIENTED_EDGE ( 'NONE', *, *, #20882, .T. ) ;
#22497 = DIRECTION ( 'NONE',  ( -0.000000000000000000, 1.000000000000000000, 3.495664435217746987E-15 ) ) ;
#22498 = DIRECTION ( 'NONE',  ( -1.000000000000000000, 0.000000000000000000, 0.000000000000000000 ) ) ;
#22499 = CARTESIAN_POINT ( 'NONE',  ( -69.99999999999997158, -87.33333333333338544, 145.0000000000000000 ) ) ;
#22500 = ITEM_DEFINED_TRANSFORMATION ( 'NONE', 'NONE', #13146,  #11210 ) ;
#22501 = ORIENTED_EDGE ( 'NONE', *, *, #21594, .T. ) ;
#22503 = CARTESIAN_POINT ( 'NONE',  ( 146.4449999999997658, -209.9999999999996874, 30.00000000000641975 ) ) ;
#22502 = VECTOR ( 'NONE', #14273, 1000.000000000000114 ) ;
#22504 = ORIENTED_EDGE ( 'NONE', *, *, #17902, .T. ) ;
#22505 = FACE_BOUND ( 'NONE', #6936, .T. ) ;
#22506 = VECTOR ( 'NONE', #9688, 1000.000000000000000 ) ;
#22507 = DIRECTION ( 'NONE',  ( 1.000000000000000000, 0.000000000000000000, 0.000000000000000000 ) ) ;
#22508 = VERTEX_POINT ( 'NONE', #19477 ) ;
#22509 = CARTESIAN_POINT ( 'NONE',  ( -44.99999999999995026, -56.79999999999969162, 102.3500000000002217 ) ) ;
#22510 = ORIENTED_EDGE ( 'NONE', *, *, #19188, .T. ) ;
#22511 = PLANE ( 'NONE',  #16164 ) ;
#22512 = CARTESIAN_POINT ( 'NONE',  ( -1.144235203016679359, -3.958177651039096911, -0.09382832055446428676 ) ) ;
#22513 = PLANE ( 'NONE',  #2672 ) ;
#22514 = PLANE ( 'NONE',  #5937 ) ;
#22515 = LINE ( 'NONE', #5864, #6498 ) ;
#22516 = DIRECTION ( 'NONE',  ( -1.000000000000000000, 0.000000000000000000, -6.982962677686266711E-15 ) ) ;
#22517 = CARTESIAN_POINT ( 'NONE',  ( -7.894955577759523280, 1.603085139988202901, -7.593799241562120272 ) ) ;
#22518 = VERTEX_POINT ( 'NONE', #6589 ) ;
#22519 = PLANE ( 'NONE',  #21130 ) ;
#22520 = CARTESIAN_POINT ( 'NONE',  ( -285.2000000000008981, 30.00000000000101963, -107.6499999999999773 ) ) ;
#22521 = ORIENTED_EDGE ( 'NONE', *, *, #3190, .T. ) ;
#22522 = EDGE_CURVE ( 'NONE', #13741, #17788, #2933, .T. ) ;
#22523 = VERTEX_POINT ( 'NONE', #10474 ) ;
#22524 = DIRECTION ( 'NONE',  ( -0.000000000000000000, -0.000000000000000000, 1.000000000000000000 ) ) ;
#22526 = CIRCLE ( 'NONE', #5554, 7.500000000000000000 ) ;
#22525 = CYLINDRICAL_SURFACE ( 'NONE', #1459, 2.500000000000002220 ) ;
#22527 = CARTESIAN_POINT ( 'NONE',  ( 40.00000000000000000, 100.0000000000000000, -150.2000000000005571 ) ) ;
#22528 = EDGE_CURVE ( 'NONE', #16299, #6312, #6697, .T. ) ;
#22529 = EDGE_LOOP ( 'NONE', ( #14584, #16689, #19180, #16426 ) ) ;
#22530 = DIRECTION ( 'NONE',  ( 0.000000000000000000, 1.000000000000000000, 0.000000000000000000 ) ) ;
#22531 = DIRECTION ( 'NONE',  ( -0.000000000000000000, -0.000000000000000000, 1.000000000000000000 ) ) ;
#22532 = ADVANCED_FACE ( 'NONE', ( #6815 ), #12650, .F. ) ;
#22533 = FACE_OUTER_BOUND ( 'NONE', #20837, .T. ) ;
#22534 = VERTEX_POINT ( 'NONE', #13004 ) ;
#22535 = CARTESIAN_POINT ( 'NONE',  ( 4.197393957002303999, -0.4069871074557456780, -3.503767560748925813 ) ) ;
#22536 = FACE_OUTER_BOUND ( 'NONE', #17496, .T. ) ;
#22537 = EDGE_CURVE ( 'NONE', #11056, #7557, #20192, .T. ) ;
#22538 = LINE ( 'NONE', #342, #15598 ) ;
#22539 = VERTEX_POINT ( 'NONE', #18266 ) ;
#22540 = CARTESIAN_POINT ( 'NONE',  ( 281.1079617568158824, 269.7223300543793698, -145.4976310729377644 ) ) ;
#22541 = CONTEXT_DEPENDENT_SHAPE_REPRESENTATION ( #5987, #10588 ) ;
#22542 = CARTESIAN_POINT ( 'NONE',  ( -20.63749999999999929, 0.000000000000000000, -19.99999999999999289 ) ) ;
#22543 = AXIS2_PLACEMENT_3D ( 'NONE', #17552, #19120, #5971 ) ;
#22544 = DIRECTION ( 'NONE',  ( 1.000000000000000000, 0.000000000000000000, 0.000000000000000000 ) ) ;
#22545 = PLANE ( 'NONE',  #3171 ) ;
#22546 = CIRCLE ( 'NONE', #4823, 2.055000000000001492 ) ;
#22547 = VECTOR ( 'NONE', #11894, 1000.000000000000000 ) ;
#22548 = ORIENTED_EDGE ( 'NONE', *, *, #288, .T. ) ;
#22549 = EDGE_LOOP ( 'NONE', ( #751, #17451, #1099, #11020 ) ) ;
#22550 = CARTESIAN_POINT ( 'NONE',  ( 3.000000000000002665, 0.000000000000000000, -23.50000000000000000 ) ) ;
#22551 = DIRECTION ( 'NONE',  ( -1.000000000000000000, 0.000000000000000000, 0.000000000000000000 ) ) ;
#22552 = VECTOR ( 'NONE', #17014, 1000.000000000000000 ) ;
#22553 = ORIENTED_EDGE ( 'NONE', *, *, #7064, .F. ) ;
#22554 = CARTESIAN_POINT ( 'NONE',  ( 287.4000000000013415, -127.0000000000000568, -146.4928932188134070 ) ) ;
#22555 = EDGE_CURVE ( 'NONE', #22523, #2480, #22018, .T. ) ;
#22556 = DIRECTION ( 'NONE',  ( 1.000000000000000000, -0.000000000000000000, 6.982962677686266711E-15 ) ) ;
#22557 = ORIENTED_EDGE ( 'NONE', *, *, #13607, .T. ) ;
#22558 = DIRECTION ( 'NONE',  ( 0.000000000000000000, -1.000000000000000000, 1.287488025362403787E-15 ) ) ;
#22559 = AXIS2_PLACEMENT_3D ( 'NONE', #12590, #19902, #1559 ) ;
#22560 = ORIENTED_EDGE ( 'NONE', *, *, #18029, .F. ) ;
#22561 = DIRECTION ( 'NONE',  ( 0.000000000000000000, 0.000000000000000000, 1.000000000000000000 ) ) ;
#22562 = ADVANCED_FACE ( 'NONE', ( #20443 ), #18831, .F. ) ;
#22563 = CARTESIAN_POINT ( 'NONE',  ( -69.99999999999997158, -112.6666666666667140, 124.9999999999999858 ) ) ;
#22564 = ORIENTED_EDGE ( 'NONE', *, *, #13318, .T. ) ;
#22565 = EDGE_LOOP ( 'NONE', ( #9455, #22678 ) ) ;
#22566 = CARTESIAN_POINT ( 'NONE',  ( -0.1756481739660520902, 4.720212674038980261, -3.469390959564065291 ) ) ;
#22567 = EDGE_CURVE ( 'NONE', #5073, #9980, #7517, .T. ) ;
#22568 = CARTESIAN_POINT ( 'NONE',  ( 0.000000000000000000, -1.178949249685218303, -2.041999999999998039 ) ) ;
#22569 = CIRCLE ( 'NONE', #23356, 2.500000000000002220 ) ;
#22570 = CARTESIAN_POINT ( 'NONE',  ( -16.51654882469417984, -1018.838720569499060, -145.0000000000001421 ) ) ;
#22571 = CARTESIAN_POINT ( 'NONE',  ( 2.500000000000000000, 0.000000000000000000, 2.041999999999999815 ) ) ;
#22572 = FACE_OUTER_BOUND ( 'NONE', #14651, .T. ) ;
#22573 = DIRECTION ( 'NONE',  ( 0.000000000000000000, 0.000000000000000000, 1.000000000000000000 ) ) ;
#22574 = EDGE_CURVE ( 'NONE', #22842, #8989, #21778, .T. ) ;
#22575 = VECTOR ( 'NONE', #22558, 1000.000000000000000 ) ;
#22576 = LINE ( 'NONE', #8223, #2678 ) ;
#22577 = EDGE_LOOP ( 'NONE', ( #5336, #13489, #2720, #2303 ) ) ;
#22578 = FACE_OUTER_BOUND ( 'NONE', #10730, .T. ) ;
#22579 = CARTESIAN_POINT ( 'NONE',  ( -105.0000000000000000, -29.99999999999998579, 3.000000000000001332 ) ) ;
#22580 = EDGE_CURVE ( 'NONE', #11487, #15145, #4186, .T. ) ;
#22581 = VECTOR ( 'NONE', #10939, 1000.000000000000000 ) ;
#22582 = ORIENTED_EDGE ( 'NONE', *, *, #23430, .T. ) ;
#22583 = CARTESIAN_POINT ( 'NONE',  ( -135.7895026000616667, -1074.740959209979792, -27.49999999999351985 ) ) ;
#22584 = CARTESIAN_POINT ( 'NONE',  ( 279.9999999999999432, 270.0000000000000000, -144.9999999999999716 ) ) ;
#22585 = ORIENTED_EDGE ( 'NONE', *, *, #14434, .F. ) ;
#22586 = DIRECTION ( 'NONE',  ( 0.000000000000000000, 0.000000000000000000, -1.000000000000000000 ) ) ;
#22587 = ORIENTED_EDGE ( 'NONE', *, *, #16781, .T. ) ;
#22588 = AXIS2_PLACEMENT_3D ( 'NONE', #992, #12159, #19579 ) ;
#22589 = CARTESIAN_POINT ( 'NONE',  ( 7.499999999999999112, -1.443375672974070323, -7.063244554130001518 ) ) ;
#22590 = CARTESIAN_POINT ( 'NONE',  ( 280.6816199723481873, 272.9663417894422537, -145.1245861693739130 ) ) ;
#22591 = ORIENTED_EDGE ( 'NONE', *, *, #18455, .T. ) ;
#22592 = ADVANCED_FACE ( 'NONE', ( #7049 ), #7246, .F. ) ;
#22593 = PLANE ( 'NONE',  #15 ) ;
#22594 = SURFACE_STYLE_FILL_AREA ( #15505 ) ;
#22595 = EDGE_LOOP ( 'NONE', ( #11778, #1005, #14343, #21273 ) ) ;
#22596 = DIRECTION ( 'NONE',  ( -1.000000000000000000, -3.469446951953617640E-16, -8.673617379884035472E-17 ) ) ;
#22597 = EDGE_CURVE ( 'NONE', #13337, #13636, #7051, .T. ) ;
#22598 = VERTEX_POINT ( 'NONE', #10838 ) ;
#22599 = LINE ( 'NONE', #20798, #3594 ) ;
#22600 = DIRECTION ( 'NONE',  ( 0.000000000000000000, 0.4999999999999990008, -0.8660254037844391517 ) ) ;
#22601 = DIRECTION ( 'NONE',  ( 0.000000000000000000, 0.000000000000000000, 1.000000000000000000 ) ) ;
#22602 = CARTESIAN_POINT ( 'NONE',  ( 1.118033988749894458, 0.000000000000000000, 23.50000000000000000 ) ) ;
#22603 = EDGE_CURVE ( 'NONE', #20079, #9726, #12786, .T. ) ;
#22604 = ORIENTED_EDGE ( 'NONE', *, *, #17747, .T. ) ;
#22605 = CARTESIAN_POINT ( 'NONE',  ( -281.3684637452625452, 268.4807971656549626, -150.1999999999999602 ) ) ;
#22606 = AXIS2_PLACEMENT_3D ( 'NONE', #10421, #19080, #2545 ) ;
#22607 = ADVANCED_FACE ( 'NONE', ( #19924 ), #22241, .F. ) ;
#22608 =( NAMED_UNIT ( * ) SI_UNIT ( $, .STERADIAN. ) SOLID_ANGLE_UNIT ( ) );
#22610 = EDGE_LOOP ( 'NONE', ( #9041, #7900 ) ) ;
#22609 = VERTEX_POINT ( 'NONE', #5711 ) ;
#22611 = CARTESIAN_POINT ( 'NONE',  ( 175.6576952185801019, -1494.741724650848937, 0.000000000000000000 ) ) ;
#22612 = DIRECTION ( 'NONE',  ( 0.000000000000000000, 0.000000000000000000, -1.000000000000000000 ) ) ;
#22613 = DIRECTION ( 'NONE',  ( -1.000000000000000000, -0.000000000000000000, -0.000000000000000000 ) ) ;
#22614 = CARTESIAN_POINT ( 'NONE',  ( 282.6188186979285888, 272.3436892194421262, 145.4976310729378497 ) ) ;
#22615 = CARTESIAN_POINT ( 'NONE',  ( -146.0000000000005400, -204.4690652294800657, -32.05499999999356930 ) ) ;
#22616 = ORIENTED_EDGE ( 'NONE', *, *, #3572, .F. ) ;
#22617 = AXIS2_PLACEMENT_3D ( 'NONE', #7010, #12605, #17507 ) ;
#22618 = CARTESIAN_POINT ( 'NONE',  ( -9.787707380959941972, 2.366756716689722317, 200.0000119999999697 ) ) ;
#22619 = VECTOR ( 'NONE', #22556, 1000.000000000000000 ) ;
#22620 = DIRECTION ( 'NONE',  ( 0.000000000000000000, 0.000000000000000000, 1.000000000000000000 ) ) ;
#22621 = CARTESIAN_POINT ( 'NONE',  ( 171.6502151485109948, 95.33502053007563859, 27.50000000000675371 ) ) ;
#22622 = EDGE_LOOP ( 'NONE', ( #19636, #18945, #2717, #1184 ) ) ;
#22623 = DIRECTION ( 'NONE',  ( 0.000000000000000000, 0.000000000000000000, -1.000000000000000000 ) ) ;
#22624 = ORIENTED_EDGE ( 'NONE', *, *, #1472, .T. ) ;
#22626 = EDGE_CURVE ( 'NONE', #14720, #13931, #3897, .T. ) ;
#22625 = FACE_BOUND ( 'NONE', #11993, .T. ) ;
#22627 = CARTESIAN_POINT ( 'NONE',  ( -52.99999999999997158, -62.00000000000001421, 5.199999999999997513 ) ) ;
#22628 = VERTEX_POINT ( 'NONE', #9713 ) ;
#22629 = DIRECTION ( 'NONE',  ( 0.000000000000000000, 0.000000000000000000, 1.000000000000000000 ) ) ;
#22630 = ORIENTED_EDGE ( 'NONE', *, *, #5297, .T. ) ;
#22631 = CARTESIAN_POINT ( 'NONE',  ( 145.0000000000000284, 0.000000000000000000, 90.00000000000000000 ) ) ;
#22632 = DIRECTION ( 'NONE',  ( -0.000000000000000000, -0.000000000000000000, 1.000000000000000000 ) ) ;
#22633 = LINE ( 'NONE', #311, #13518 ) ;
#22634 = DIRECTION ( 'NONE',  ( 0.000000000000000000, -2.618450529776313049E-15, -1.000000000000000000 ) ) ;
#22635 = EDGE_CURVE ( 'NONE', #5897, #17167, #23181, .T. ) ;
#22636 = DIRECTION ( 'NONE',  ( 0.000000000000000000, 0.000000000000000000, -1.000000000000000000 ) ) ;
#22637 = CARTESIAN_POINT ( 'NONE',  ( -4.250000000000000000, 5.204748896376250699E-16, -0.5251556536572846712 ) ) ;
#22638 = AXIS2_PLACEMENT_3D ( 'NONE', #13425, #22907, #2627 ) ;
#22639 = CARTESIAN_POINT ( 'NONE',  ( -7.499999999999999112, 4.651022038490018495, -7.928862870699868282 ) ) ;
#22640 = EDGE_CURVE ( 'NONE', #7088, #2989, #18821, .T. ) ;
#22641 = ORIENTED_EDGE ( 'NONE', *, *, #11867, .F. ) ;
#22642 = CARTESIAN_POINT ( 'NONE',  ( 0.000000000000000000, 0.000000000000000000, -100.0000000000000000 ) ) ;
#22643 = VECTOR ( 'NONE', #10098, 1000.000000000000114 ) ;
#22644 = CARTESIAN_POINT ( 'NONE',  ( -129.6400180686271142, -1072.557589128678273, -32.49999999999356959 ) ) ;
#22645 = AXIS2_PLACEMENT_3D ( 'NONE', #14366, #6974, #19755 ) ;
#22646 = VERTEX_POINT ( 'NONE', #13484 ) ;
#22647 = ORIENTED_EDGE ( 'NONE', *, *, #14352, .F. ) ;
#22648 = DIRECTION ( 'NONE',  ( -0.000000000000000000, -0.000000000000000000, -1.000000000000000000 ) ) ;
#22649 = CYLINDRICAL_SURFACE ( 'NONE', #19209, 2.200000000000028155 ) ;
#22650 = CARTESIAN_POINT ( 'NONE',  ( -123.1824219776882927, 83.04955713735503764, 27.50000000000641975 ) ) ;
#22651 = ORIENTED_EDGE ( 'NONE', *, *, #17627, .T. ) ;
#22652 = LINE ( 'NONE', #22419, #2631 ) ;
#22653 = LINE ( 'NONE', #7938, #3157 ) ;
#22654 = AXIS2_PLACEMENT_3D ( 'NONE', #17689, #3184, #1153 ) ;
#22655 = CARTESIAN_POINT ( 'NONE',  ( 0.000000000000000000, 0.000000000000000000, 0.000000000000000000 ) ) ;
#22656 = ORIENTED_EDGE ( 'NONE', *, *, #19583, .T. ) ;
#22657 = CARTESIAN_POINT ( 'NONE',  ( 280.7154581756738594, 271.5968359015654983, 148.5570580646227370 ) ) ;
#22658 = CARTESIAN_POINT ( 'NONE',  ( 100.0000000000000000, -1400.000000000000000, 124.9999999999998295 ) ) ;
#22659 = CONICAL_SURFACE ( 'NONE', #1826, 2.055000000000001492, 0.7853981633974633780 ) ;
#22660 = UNCERTAINTY_MEASURE_WITH_UNIT (LENGTH_MEASURE( 1.000000000000000082E-05 ), #3030, 'distance_accuracy_value', 'NONE');
#22661 = FACE_BOUND ( 'NONE', #21380, .T. ) ;
#22662 = AXIS2_PLACEMENT_3D ( 'NONE', #13389, #13524, #8040 ) ;
#22663 = ORIENTED_EDGE ( 'NONE', *, *, #19631, .T. ) ;
#22664 = CARTESIAN_POINT ( 'NONE',  ( 65.00000000000004263, -56.79999999999959925, 65.00000000000019895 ) ) ;
#22665 = DIRECTION ( 'NONE',  ( 0.000000000000000000, 0.000000000000000000, 1.000000000000000000 ) ) ;
#22666 =( REPRESENTATION_RELATIONSHIP ('NONE','NONE', #10127, #5587 ) REPRESENTATION_RELATIONSHIP_WITH_TRANSFORMATION ( #9461 )SHAPE_REPRESENTATION_RELATIONSHIP( ) );
#22667 = FACE_OUTER_BOUND ( 'NONE', #5088, .T. ) ;
#22668 = CARTESIAN_POINT ( 'NONE',  ( -7.703011046602857601E-15, -132.2000000000000455, 146.4928932188134638 ) ) ;
#22669 = ADVANCED_FACE ( 'NONE', ( #15269, #17619 ), #2327, .T. ) ;
#22670 = ORIENTED_EDGE ( 'NONE', *, *, #12775, .F. ) ;
#22671 = ORIENTED_EDGE ( 'NONE', *, *, #17978, .F. ) ;
#22672 = CARTESIAN_POINT ( 'NONE',  ( -44.99999999999997868, -56.79999999999938609, 137.3500000000001648 ) ) ;
#22673 = DIRECTION ( 'NONE',  ( -0.5000000000000019984, -0.8660254037844375974, 0.000000000000000000 ) ) ;
#22674 = VECTOR ( 'NONE', #9361, 1000.000000000000000 ) ;
#22675 = AXIS2_PLACEMENT_3D ( 'NONE', #9550, #15126, #22455 ) ;
#22676 = AXIS2_PLACEMENT_3D ( 'NONE', #11715, #8065, #7816 ) ;
#22677 = VECTOR ( 'NONE', #418, 1000.000000000000000 ) ;
#22678 = ORIENTED_EDGE ( 'NONE', *, *, #12473, .T. ) ;
#22679 = FACE_OUTER_BOUND ( 'NONE', #22746, .T. ) ;
#22680 = AXIS2_PLACEMENT_3D ( 'NONE', #21566, #5031, #10600 ) ;
#22681 = CARTESIAN_POINT ( 'NONE',  ( -126.6049454172962214, 89.42142849840972474, 31.11216498479349468 ) ) ;
#22682 = EDGE_LOOP ( 'NONE', ( #20002, #18571, #10999, #20625 ) ) ;
#22683 = CARTESIAN_POINT ( 'NONE',  ( 2.500000000000000000, 1.178949249685213863, -2.042000000000001148 ) ) ;
#22684 = ORIENTED_EDGE ( 'NONE', *, *, #6868, .F. ) ;
#22685 = CYLINDRICAL_SURFACE ( 'NONE', #4835, 5.000000000000001776 ) ;
#22686 = CARTESIAN_POINT ( 'NONE',  ( 146.4449999999998226, -801.0618695410399823, 27.50000000000642331 ) ) ;
#22687 = ORIENTED_EDGE ( 'NONE', *, *, #19584, .T. ) ;
#22688 = ORIENTED_EDGE ( 'NONE', *, *, #13603, .F. ) ;
#22689 = CARTESIAN_POINT ( 'NONE',  ( 3.453038570460273071, 2.625189405340834448, -3.535263753543585352 ) ) ;
#22690 = CIRCLE ( 'NONE', #9215, 2.499999999999998668 ) ;
#22691 = DIRECTION ( 'NONE',  ( -1.350636282998972974E-14, 0.000000000000000000, -1.000000000000000000 ) ) ;
#22693 = AXIS2_PLACEMENT_3D ( 'NONE', #2937, #8282, #16008 ) ;
#22692 = PRESENTATION_LAYER_ASSIGNMENT (  '', '', ( #21614 ) ) ;
#22694 = AXIS2_PLACEMENT_3D ( 'NONE', #8159, #23219, #13737 ) ;
#22695 = AXIS2_PLACEMENT_3D ( 'NONE', #7323, #3801, #5752 ) ;
#22696 = DIRECTION ( 'NONE',  ( 0.000000000000000000, -0.8660254037844390407, -0.4999999999999992784 ) ) ;
#22697 = CARTESIAN_POINT ( 'NONE',  ( 5.276765049035074817, -6.073111908730307817, -7.634085501268428331 ) ) ;
#22698 = CIRCLE ( 'NONE', #14637, 2.650000000000041211 ) ;
#22699 = EDGE_CURVE ( 'NONE', #19505, #6984, #9830, .T. ) ;
#22700 = DIRECTION ( 'NONE',  ( -1.000000000000000000, 0.000000000000000000, 0.000000000000000000 ) ) ;
#22701 = ORIENTED_EDGE ( 'NONE', *, *, #22603, .T. ) ;
#22702 = CARTESIAN_POINT ( 'NONE',  ( 0.04725809328185039127, -9.175759667312528123, -8.057670357645362103 ) ) ;
#22703 = AXIS2_PLACEMENT_3D ( 'NONE', #6607, #14113, #1517 ) ;
#22704 = ORIENTED_EDGE ( 'NONE', *, *, #22003, .T. ) ;
#22705 = DIRECTION ( 'NONE',  ( 1.000000000000000000, 0.000000000000000000, 0.000000000000000000 ) ) ;
#22706 = CARTESIAN_POINT ( 'NONE',  ( 0.000000000000000000, -1000.000000000000000, 124.9999999999998579 ) ) ;
#22707 = EDGE_CURVE ( 'NONE', #17333, #5510, #19542, .T. ) ;
#22708 = EDGE_CURVE ( 'NONE', #23406, #4707, #1476, .T. ) ;
#22709 = ORIENTED_EDGE ( 'NONE', *, *, #12074, .T. ) ;
#22710 =( GEOMETRIC_REPRESENTATION_CONTEXT ( 3 ) GLOBAL_UNCERTAINTY_ASSIGNED_CONTEXT ( ( #4372 ) ) GLOBAL_UNIT_ASSIGNED_CONTEXT ( ( #12426, #10473, #4658 ) ) REPRESENTATION_CONTEXT ( 'NONE', 'WORKASPACE' ) );
#22711 = CARTESIAN_POINT ( 'NONE',  ( -19.87444003266270087, -15.25452100728112015, -145.0000000000000000 ) ) ;
#22712 = VECTOR ( 'NONE', #13721, 1000.000000000000000 ) ;
#22713 = ORIENTED_EDGE ( 'NONE', *, *, #8610, .F. ) ;
#22714 = AXIS2_PLACEMENT_3D ( 'NONE', #8041, #4855, #14412 ) ;
#22715 = CARTESIAN_POINT ( 'NONE',  ( 0.000000000000000000, -1000.000000000000000, 90.00000000000000000 ) ) ;
#22716 = LINE ( 'NONE', #7875, #4938 ) ;
#22717 = AXIS2_PLACEMENT_3D ( 'NONE', #4117, #9460, #7878 ) ;
#22718 = CIRCLE ( 'NONE', #5261, 2.499999999999998668 ) ;
#22719 = EDGE_LOOP ( 'NONE', ( #11369, #10294, #19609, #5759 ) ) ;
#22720 = EDGE_CURVE ( 'NONE', #21618, #3982, #19987, .T. ) ;
#22721 = FACE_OUTER_BOUND ( 'NONE', #34, .T. ) ;
#22722 = DIRECTION ( 'NONE',  ( -0.000000000000000000, -0.000000000000000000, 1.000000000000000000 ) ) ;
#22723 = EDGE_LOOP ( 'NONE', ( #9010, #5425, #4787, #8053 ) ) ;
#22724 = CARTESIAN_POINT ( 'NONE',  ( 0.000000000000000000, 5.173457871231061435E-13, 150.2000000000009550 ) ) ;
#22725 = DIRECTION ( 'NONE',  ( -0.7232617928448825673, 0.6905739489807055653, 6.982962677686265922E-15 ) ) ;
#22726 = CARTESIAN_POINT ( 'NONE',  ( 20.00000000000000000, 0.000000000000000000, -138.9999999999999716 ) ) ;
#22727 = CARTESIAN_POINT ( 'NONE',  ( 45.00000000000002132, -52.79999999999935767, 142.6500000000002046 ) ) ;
#22728 = ORIENTED_EDGE ( 'NONE', *, *, #11663, .F. ) ;
#22729 = AXIS2_PLACEMENT_3D ( 'NONE', #6912, #19453, #21517 ) ;
#22730 = CARTESIAN_POINT ( 'NONE',  ( -281.1021437883072736, 269.7094021484634254, 145.4974534559950712 ) ) ;
#22731 =( GEOMETRIC_REPRESENTATION_CONTEXT ( 3 ) GLOBAL_UNCERTAINTY_ASSIGNED_CONTEXT ( ( #13828 ) ) GLOBAL_UNIT_ASSIGNED_CONTEXT ( ( #11673, #21042, #7891 ) ) REPRESENTATION_CONTEXT ( 'NONE', 'WORKASPACE' ) );
#22732 = VECTOR ( 'NONE', #6915, 1000.000000000000000 ) ;
#22733 = VECTOR ( 'NONE', #18585, 1000.000000000000000 ) ;
#22734 = VECTOR ( 'NONE', #20851, 1000.000000000000000 ) ;
#22736 = ORIENTED_EDGE ( 'NONE', *, *, #19162, .F. ) ;
#22735 = ORIENTED_EDGE ( 'NONE', *, *, #6445, .F. ) ;
#22737 = B_SPLINE_CURVE_WITH_KNOTS ( 'NONE', 3,
 ( #11942, #23232, #8389, #2726, #17457, #899, #15771, #6590, #19480, #6703, #1147, #15657, #22985, #13990, #4769, #5366 ),
 .UNSPECIFIED., .F., .F.,
 ( 4, 2, 2, 2, 2, 2, 2, 4 ),
 ( 0.000000000000000000, 0.0009361184303671995577, 0.001404177645550716991, 0.001872236860734234534, 0.002340296075917751642, 0.002808355291101269184, 0.003276414506284786726, 0.003744473721468304268 ),
 .UNSPECIFIED. ) ;
#22738 = CARTESIAN_POINT ( 'NONE',  ( 376.7679829879423323, -634.3897061142869234, 0.000000000000000000 ) ) ;
#22739 = CARTESIAN_POINT ( 'NONE',  ( 1.411581201560190495E-15, 4.862606272033091592, -3.745885042887436622 ) ) ;
#22740 = CARTESIAN_POINT ( 'NONE',  ( 2.700000000000001510, 0.000000000000000000, 0.000000000000000000 ) ) ;
#22741 = EDGE_CURVE ( 'NONE', #4158, #16275, #19421, .T. ) ;
#22742 = ADVANCED_FACE ( 'NONE', ( #4266, #17186, #21367, #11421, #15029 ), #9586, .T. ) ;
#22743 = CARTESIAN_POINT ( 'NONE',  ( 282.1999999999999318, 268.0880230824753312, 146.3684665479256068 ) ) ;
#22744 = DIRECTION ( 'NONE',  ( 1.000000000000000000, 0.000000000000000000, 0.000000000000000000 ) ) ;
#22745 = EDGE_CURVE ( 'NONE', #5068, #11184, #281, .T. ) ;
#22746 = EDGE_LOOP ( 'NONE', ( #15678, #6499, #6524, #12006 ) ) ;
#22747 = CARTESIAN_POINT ( 'NONE',  ( -2.999999999999998668, 0.000000000000000000, -20.30000000000000071 ) ) ;
#22748 = ADVANCED_FACE ( 'NONE', ( #22376 ), #13872, .F. ) ;
#22749 = EDGE_CURVE ( 'NONE', #22534, #9214, #21261, .T. ) ;
#22750 = AXIS2_PLACEMENT_3D ( 'NONE', #18597, #18489, #7256 ) ;
#22751 = DIRECTION ( 'NONE',  ( 0.000000000000000000, -1.000000000000000000, 0.000000000000000000 ) ) ;
#22752 = ADVANCED_FACE ( 'NONE', ( #4001 ), #2191, .T. ) ;
#22753 = CARTESIAN_POINT ( 'NONE',  ( 124.2735041650581422, -1092.634345841123377, 27.51597717546058064 ) ) ;
#22754 =( GEOMETRIC_REPRESENTATION_CONTEXT ( 3 ) GLOBAL_UNCERTAINTY_ASSIGNED_CONTEXT ( ( #9946 ) ) GLOBAL_UNIT_ASSIGNED_CONTEXT ( ( #2539, #13699, #9696 ) ) REPRESENTATION_CONTEXT ( 'NONE', 'WORKASPACE' ) );
#22755 = AXIS2_PLACEMENT_3D ( 'NONE', #9840, #4275, #11199 ) ;
#22756 = CONTEXT_DEPENDENT_SHAPE_REPRESENTATION ( #10353, #19908 ) ;
#22757 = EDGE_LOOP ( 'NONE', ( #533, #13839, #14568, #17261 ) ) ;
#22758 = CIRCLE ( 'NONE', #12403, 20.00000000000000000 ) ;
#22759 = CIRCLE ( 'NONE', #14315, 25.00000000000000000 ) ;
#22760 = CARTESIAN_POINT ( 'NONE',  ( 4.250000000000000000, 0.000000000000000000, -9.449444346342714240 ) ) ;
#22761 = ORIENTED_EDGE ( 'NONE', *, *, #23452, .F. ) ;
#22762 = CARTESIAN_POINT ( 'NONE',  ( 60.00000000000000000, -137.1994082814340743, -2.400000000000046096 ) ) ;
#22763 = DIRECTION ( 'NONE',  ( -1.000000000000000000, 3.495664435217746987E-15, 0.000000000000000000 ) ) ;
#22764 = VERTEX_POINT ( 'NONE', #22485 ) ;
#22765 = CARTESIAN_POINT ( 'NONE',  ( -93.00000000000000000, -152.9999999999996874, 129.9038105676659711 ) ) ;
#22766 = ORIENTED_EDGE ( 'NONE', *, *, #16077, .F. ) ;
#22767 = LINE ( 'NONE', #7548, #21931 ) ;
#22768 = CARTESIAN_POINT ( 'NONE',  ( 57.99999999999999289, 0.000000000000000000, 0.000000000000000000 ) ) ;
#22769 = DIRECTION ( 'NONE',  ( -1.000000000000000000, -0.000000000000000000, -0.000000000000000000 ) ) ;
#22770 = DIRECTION ( 'NONE',  ( -1.000000000000000000, 0.000000000000000000, 0.000000000000000000 ) ) ;
#22771 = DIRECTION ( 'NONE',  ( -0.000000000000000000, -0.000000000000000000, 1.000000000000000000 ) ) ;
#22772 = CARTESIAN_POINT ( 'NONE',  ( 5.000000000000000000, 0.000000000000000000, 0.000000000000000000 ) ) ;
#22773 = CARTESIAN_POINT ( 'NONE',  ( -24.20041621714725721, 6.482064212728078090, 145.0000119999999697 ) ) ;
#22774 = ORIENTED_EDGE ( 'NONE', *, *, #2551, .T. ) ;
#22775 = VECTOR ( 'NONE', #3050, 1000.000000000000000 ) ;
#22776 = FACE_BOUND ( 'NONE', #20502, .T. ) ;
#22777 = CARTESIAN_POINT ( 'NONE',  ( -146.0000000000004832, -494.4690652294800657, -27.94499999999356632 ) ) ;
#22778 = EDGE_LOOP ( 'NONE', ( #14192, #14622, #22104, #14827 ) ) ;
#22779 = VERTEX_POINT ( 'NONE', #12120 ) ;
#22780 = LINE ( 'NONE', #16862, #20007 ) ;
#22781 = LINE ( 'NONE', #13180, #5329 ) ;
#22783 = CARTESIAN_POINT ( 'NONE',  ( -1.500000000000000000, 0.000000000000000000, 0.000000000000000000 ) ) ;
#22782 = PRODUCT_DEFINITION_SHAPE ( 'NONE', 'NONE',  #23841 ) ;
#22784 = VERTEX_POINT ( 'NONE', #2877 ) ;
#22785 = EDGE_CURVE ( 'NONE', #3630, #14436, #10368, .T. ) ;
#22786 = DIRECTION ( 'NONE',  ( 1.000000000000000000, 0.000000000000000000, 0.000000000000000000 ) ) ;
#22787 = EDGE_CURVE ( 'NONE', #7773, #18735, #527, .T. ) ;
#22788 = CARTESIAN_POINT ( 'NONE',  ( 70.00000000000000000, -112.6666666666666714, 148.0000000000000000 ) ) ;
#22789 = CARTESIAN_POINT ( 'NONE',  ( 2.500000000000000000, 1.178949249685217415, 2.041999999999998483 ) ) ;
#22790 = ORIENTED_EDGE ( 'NONE', *, *, #20025, .F. ) ;
#22791 = CARTESIAN_POINT ( 'NONE',  ( 281.3681929792552410, 268.4822561791010571, 150.1663407402829762 ) ) ;
#22792 = DIRECTION ( 'NONE',  ( -0.000000000000000000, -0.000000000000000000, 1.000000000000000000 ) ) ;
#22793 = FILL_AREA_STYLE ('',( #14007 ) ) ;
#22794 = ORIENTED_EDGE ( 'NONE', *, *, #23057, .F. ) ;
#22795 = CARTESIAN_POINT ( 'NONE',  ( 282.1696999999999775, 267.7999999999999545, -146.4928932188133786 ) ) ;
#22796 = CARTESIAN_POINT ( 'NONE',  ( -194.7500000000004832, -204.4690652294793836, -29.99999999999322498 ) ) ;
#22797 = DIRECTION ( 'NONE',  ( -0.000000000000000000, -0.000000000000000000, 1.000000000000000000 ) ) ;
#22798 = CYLINDRICAL_SURFACE ( 'NONE', #12880, 2.649999999999971934 ) ;
#22799 = UNCERTAINTY_MEASURE_WITH_UNIT (LENGTH_MEASURE( 1.000000000000000082E-05 ), #6970, 'distance_accuracy_value', 'NONE');
#22800 = ORIENTED_EDGE ( 'NONE', *, *, #13492, .T. ) ;
#22801 = ORIENTED_EDGE ( 'NONE', *, *, #16705, .F. ) ;
#22802 = FACE_OUTER_BOUND ( 'NONE', #12091, .T. ) ;
#22803 = DIRECTION ( 'NONE',  ( 0.000000000000000000, 0.000000000000000000, -1.000000000000000000 ) ) ;
#22804 =( REPRESENTATION_RELATIONSHIP ('NONE','NONE', #10127, #18083 ) REPRESENTATION_RELATIONSHIP_WITH_TRANSFORMATION ( #5969 )SHAPE_REPRESENTATION_RELATIONSHIP( ) );
#22805 = EDGE_LOOP ( 'NONE', ( #4914, #16401, #15216, #21362 ) ) ;
#22806 = FACE_OUTER_BOUND ( 'NONE', #23376, .T. ) ;
#22807 = DIRECTION ( 'NONE',  ( 0.000000000000000000, -1.000000000000000000, -3.172065784643303781E-15 ) ) ;
#22808 = ORIENTED_EDGE ( 'NONE', *, *, #19898, .T. ) ;
#22809 = PLANE ( 'NONE',  #12225 ) ;
#22810 = ORIENTED_EDGE ( 'NONE', *, *, #12775, .T. ) ;
#22811 = DIRECTION ( 'NONE',  ( -0.000000000000000000, 1.471414886128461471E-15, 1.000000000000000000 ) ) ;
#22812 = DIRECTION ( 'NONE',  ( -0.000000000000000000, 0.000000000000000000, 1.000000000000000000 ) ) ;
#22813 = ORIENTED_EDGE ( 'NONE', *, *, #5618, .T. ) ;
#22814 = ORIENTED_EDGE ( 'NONE', *, *, #8713, .T. ) ;
#22815 = CARTESIAN_POINT ( 'NONE',  ( 3.472371940585993855, 2.614027278893175321, -3.320322319201766792 ) ) ;
#22816 = DIRECTION ( 'NONE',  ( 0.000000000000000000, 0.000000000000000000, 1.000000000000000000 ) ) ;
#22817 = DIRECTION ( 'NONE',  ( 0.000000000000000000, 0.000000000000000000, -1.000000000000000000 ) ) ;
#22818 = DIRECTION ( 'NONE',  ( -1.000000000000000000, -0.000000000000000000, -0.000000000000000000 ) ) ;
#22819 = ORIENTED_EDGE ( 'NONE', *, *, #7650, .F. ) ;
#22820 = CARTESIAN_POINT ( 'NONE',  ( -1.060314165522979968, -8.048081368954337123, -7.659344964963557878 ) ) ;
#22821 = ORIENTED_EDGE ( 'NONE', *, *, #4599, .T. ) ;
#22822 = ADVANCED_BREP_SHAPE_REPRESENTATION ( '', ( #12018, #11210 ), #22731 ) ;
#22823 = CARTESIAN_POINT ( 'NONE',  ( 1.391697335622810172, 4.043246145443375461, -3.503898532754365913 ) ) ;
#22824 = EDGE_CURVE ( 'NONE', #16291, #1461, #3491, .T. ) ;
#22825 = CIRCLE ( 'NONE', #9752, 25.00000000000000000 ) ;
#22826 = EDGE_LOOP ( 'NONE', ( #5059, #2215, #18931, #20484 ) ) ;
#22827 = CARTESIAN_POINT ( 'NONE',  ( -24.84002319583889573, -3.266795291467043061, -145.0000000000000284 ) ) ;
#22828 = ORIENTED_EDGE ( 'NONE', *, *, #4827, .F. ) ;
#22829 = CYLINDRICAL_SURFACE ( 'NONE', #22146, 2.500000000000000444 ) ;
#22830 = DIRECTION ( 'NONE',  ( 0.000000000000000000, 0.000000000000000000, 1.000000000000000000 ) ) ;
#22831 = VERTEX_POINT ( 'NONE', #16193 ) ;
#22832 = ADVANCED_FACE ( 'NONE', ( #14284 ), #12721, .F. ) ;
#22833 = CARTESIAN_POINT ( 'NONE',  ( -281.3684637172360112, 268.4847249064868606, 150.2299999999999898 ) ) ;
#22834 = ADVANCED_FACE ( 'NONE', ( #7114 ), #1672, .T. ) ;
#22835 = EDGE_LOOP ( 'NONE', ( #6184, #14761 ) ) ;
#22836 = DIRECTION ( 'NONE',  ( -0.000000000000000000, -0.000000000000000000, 1.000000000000000000 ) ) ;
#22837 = CARTESIAN_POINT ( 'NONE',  ( -15.25452100747948769, -980.1255599675661188, -145.0000000000001421 ) ) ;
#22838 = EDGE_CURVE ( 'NONE', #19530, #4707, #10898, .T. ) ;
#22839 = CARTESIAN_POINT ( 'NONE',  ( -6.601567268551443490, 5.319966374295965750, -7.792327460285856766 ) ) ;
#22840 = VECTOR ( 'NONE', #8668, 1000.000000000000000 ) ;
#22841 = DIRECTION ( 'NONE',  ( -0.000000000000000000, 1.000000000000000000, -3.469446951953613794E-15 ) ) ;
#22842 = VERTEX_POINT ( 'NONE', #16069 ) ;
#22843 = CARTESIAN_POINT ( 'NONE',  ( 51.87806360044913134, -135.4018704341552564, -90.00000000000000000 ) ) ;
#22845 = VERTEX_POINT ( 'NONE', #12841 ) ;
#22844 = ORIENTED_EDGE ( 'NONE', *, *, #18547, .T. ) ;
#22846 = DIRECTION ( 'NONE',  ( 0.7232617928448825673, -0.6905739489807055653, -6.982962677686266711E-15 ) ) ;
#22847 = CARTESIAN_POINT ( 'NONE',  ( 7.500000000000000000, -3.202733125947433201, -7.213074474936314928 ) ) ;
#22848 = DIRECTION ( 'NONE',  ( 0.000000000000000000, 0.000000000000000000, 1.000000000000000000 ) ) ;
#22849 = CARTESIAN_POINT ( 'NONE',  ( 72.64999999999999147, -112.6666666666666714, 148.0000000000000000 ) ) ;
#22850 = CARTESIAN_POINT ( 'NONE',  ( -280.0000000000000568, 269.9696999999999889, -144.9999999999999716 ) ) ;
#22851 = ORIENTED_EDGE ( 'NONE', *, *, #4425, .T. ) ;
#22852 = AXIS2_PLACEMENT_3D ( 'NONE', #16855, #15306, #318 ) ;
#22853 = DIRECTION ( 'NONE',  ( 0.000000000000000000, 0.000000000000000000, -1.000000000000000000 ) ) ;
#22854 = DIRECTION ( 'NONE',  ( 0.000000000000000000, 0.000000000000000000, 1.000000000000000000 ) ) ;
#22855 = DIRECTION ( 'NONE',  ( 0.000000000000000000, 1.000000000000000000, 0.000000000000000000 ) ) ;
#22856 = ITEM_DEFINED_TRANSFORMATION ( 'NONE', 'NONE', #20044,  #11210 ) ;
#22857 = ORIENTED_EDGE ( 'NONE', *, *, #994, .T. ) ;
#22858 = CARTESIAN_POINT ( 'NONE',  ( 80.00000000000001421, -59.79999999999998295, 5.199999999999996625 ) ) ;
#22859 = EDGE_CURVE ( 'NONE', #22100, #17297, #23071, .T. ) ;
#22860 = ORIENTED_EDGE ( 'NONE', *, *, #22120, .F. ) ;
#22861 = LINE ( 'NONE', #13983, #11594 ) ;
#22862 = CARTESIAN_POINT ( 'NONE',  ( 0.000000000000000000, 0.000000000000000000, 138.9999999999999716 ) ) ;
#22863 = EDGE_LOOP ( 'NONE', ( #11743, #23241, #20667, #15452 ) ) ;
#22864 = CARTESIAN_POINT ( 'NONE',  ( -25.00004926069054889, 1.642023387880738872, -145.0000000000000000 ) ) ;
#22865 = ADVANCED_FACE ( 'NONE', ( #23765 ), #22294, .T. ) ;
#22866 = EDGE_LOOP ( 'NONE', ( #7631, #19003, #12015, #11380 ) ) ;
#22867 = DIRECTION ( 'NONE',  ( 0.000000000000000000, 0.000000000000000000, 1.000000000000000000 ) ) ;
#22868 = EDGE_CURVE ( 'NONE', #10543, #10801, #12601, .T. ) ;
#22869 = CARTESIAN_POINT ( 'NONE',  ( 0.000000000000000000, 0.000000000000000000, 90.00000000000000000 ) ) ;
#22870 = AXIS2_PLACEMENT_3D ( 'NONE', #23111, #6587, #4523 ) ;
#22871 = LINE ( 'NONE', #9984, #21379 ) ;
#22872 = DIRECTION ( 'NONE',  ( -0.000000000000000000, 0.000000000000000000, -1.000000000000000000 ) ) ;
#22873 = B_SPLINE_CURVE_WITH_KNOTS ( 'NONE', 3,
 ( #21598, #14254, #933, #23023, #15815, #2976, #23162, #12341, #6625, #19650, #8674, #3112, #17849, #5061, #12466, #6492 ),
 .UNSPECIFIED., .F., .F.,
 ( 4, 2, 2, 2, 2, 2, 2, 4 ),
 ( 2.775557561562891351E-17, 0.0009361184303670230496, 0.001404177645550584719, 0.001872236860734146496, 0.002340296075917707840, 0.002808355291101269618, 0.003276414506284831395, 0.003744473721468393173 ),
 .UNSPECIFIED. ) ;
#22874 = CARTESIAN_POINT ( 'NONE',  ( 40.00000000000000000, 100.0000000000000000, 150.2000000000009550 ) ) ;
#22875 = DIRECTION ( 'NONE',  ( 0.000000000000000000, 0.000000000000000000, 1.000000000000000000 ) ) ;
#22876 = EDGE_CURVE ( 'NONE', #11798, #10962, #15774, .T. ) ;
#22877 = VERTEX_POINT ( 'NONE', #21730 ) ;
#22878 = ADVANCED_FACE ( 'NONE', ( #19791, #21959 ), #12715, .T. ) ;
#22879 = SURFACE_STYLE_USAGE ( .BOTH. , #11585 ) ;
#22880 = CYLINDRICAL_SURFACE ( 'NONE', #13844, 20.00000000000000000 ) ;
#22881 = CARTESIAN_POINT ( 'NONE',  ( -110.0000000000000000, -94.99999999999997158, 3.000000000000000000 ) ) ;
#22882 = ORIENTED_EDGE ( 'NONE', *, *, #22197, .F. ) ;
#22883 = ORIENTED_EDGE ( 'NONE', *, *, #1724, .F. ) ;
#22884 = CARTESIAN_POINT ( 'NONE',  ( 158.0000000000000568, -557.0000000000000000, -57.00000000000000000 ) ) ;
#22885 = DIRECTION ( 'NONE',  ( 1.000000000000000000, 0.000000000000000000, 0.000000000000000000 ) ) ;
#22886 = CARTESIAN_POINT ( 'NONE',  ( -282.2000000000013529, -89.99999999999896261, -40.33333333333332860 ) ) ;
#22887 = CIRCLE ( 'NONE', #2057, 2.649999999999985700 ) ;
#22888 = AXIS2_PLACEMENT_3D ( 'NONE', #1641, #19641, #23623 ) ;
#22889 = DIRECTION ( 'NONE',  ( 0.000000000000000000, -1.000000000000000000, -0.000000000000000000 ) ) ;
#22890 = CARTESIAN_POINT ( 'NONE',  ( -140.0355749532211007, 37.61698748598567477, -2.775557561562891351E-14 ) ) ;
#22891 = CARTESIAN_POINT ( 'NONE',  ( -2.699999999999997513, 0.000000000000000000, -19.99999999999999645 ) ) ;
#22892 = ORIENTED_EDGE ( 'NONE', *, *, #2575, .F. ) ;
#22893 = CARTESIAN_POINT ( 'NONE',  ( 158.0000000000000284, -500.0000000000000000, 30.00000000000001421 ) ) ;
#22894 = DIRECTION ( 'NONE',  ( 0.000000000000000000, 0.8660254037844380415, -0.5000000000000009992 ) ) ;
#22895 = DIRECTION ( 'NONE',  ( 1.000000000000000000, -0.000000000000000000, -0.000000000000000000 ) ) ;
#22896 = ORIENTED_EDGE ( 'NONE', *, *, #22276, .T. ) ;
#22897 = CARTESIAN_POINT ( 'NONE',  ( 280.5758453455903805, 269.9427398886703031, -145.2488155364688680 ) ) ;
#22898 = CONTEXT_DEPENDENT_SHAPE_REPRESENTATION ( #14194, #10174 ) ;
#22899 = DIRECTION ( 'NONE',  ( -1.110223024625155594E-14, 0.000000000000000000, -1.000000000000000000 ) ) ;
#22900 = LINE ( 'NONE', #4444, #20380 ) ;
#22901 = CARTESIAN_POINT ( 'NONE',  ( -284.6728700860325603, 270.1062614524586252, 146.0570750465944343 ) ) ;
#22902 = VECTOR ( 'NONE', #6839, 1000.000000000000000 ) ;
#22903 = ORIENTED_EDGE ( 'NONE', *, *, #59, .T. ) ;
#22904 = AXIS2_PLACEMENT_3D ( 'NONE', #14792, #15153, #9237 ) ;
#22906 = ORIENTED_EDGE ( 'NONE', *, *, #10634, .T. ) ;
#22905 = EDGE_CURVE ( 'NONE', #21032, #3554, #11550, .T. ) ;
#22907 = DIRECTION ( 'NONE',  ( -1.000000000000000000, -0.000000000000000000, -0.000000000000000000 ) ) ;
#22908 = LINE ( 'NONE', #6381, #12389 ) ;
#22909 = EDGE_CURVE ( 'NONE', #19218, #629, #19912, .T. ) ;
#22910 = ORIENTED_EDGE ( 'NONE', *, *, #23771, .T. ) ;
#22911 = VECTOR ( 'NONE', #10904, 1000.000000000000000 ) ;
#22912 = EDGE_LOOP ( 'NONE', ( #19632, #7385, #564 ) ) ;
#22913 = DIRECTION ( 'NONE',  ( -1.000000000000000000, 0.000000000000000000, 0.000000000000000000 ) ) ;
#22914 = CARTESIAN_POINT ( 'NONE',  ( -127.8094121079452776, 87.69139705313205013, 32.50000000000647304 ) ) ;
#22916 = VERTEX_POINT ( 'NONE', #4951 ) ;
#22915 = AXIS2_PLACEMENT_3D ( 'NONE', #11684, #16970, #15167 ) ;
#22917 = FACE_OUTER_BOUND ( 'NONE', #5208, .T. ) ;
#22918 = VERTEX_POINT ( 'NONE', #21624 ) ;
#22919 = VECTOR ( 'NONE', #244, 1000.000000000000000 ) ;
#22920 = CARTESIAN_POINT ( 'NONE',  ( -145.0000000000000284, -1000.000000000000000, 90.00000000000000000 ) ) ;
#22921 = FACE_BOUND ( 'NONE', #20367, .T. ) ;
#22922 = VERTEX_POINT ( 'NONE', #14611 ) ;
#22923 = EDGE_LOOP ( 'NONE', ( #6628, #6128, #21829, #2796 ) ) ;
#22924 = LINE ( 'NONE', #6396, #10830 ) ;
#22925 = AXIS2_PLACEMENT_3D ( 'NONE', #23369, #17825, #18181 ) ;
#22926 = CARTESIAN_POINT ( 'NONE',  ( -0.1404048886732797152, -4.699864953788083888, -3.686887068327043160 ) ) ;
#22927 = CARTESIAN_POINT ( 'NONE',  ( 4.999999999999997335, 0.000000000000000000, 4.250000000000000000 ) ) ;
#22928 = DIRECTION ( 'NONE',  ( 0.000000000000000000, 0.000000000000000000, -1.000000000000000000 ) ) ;
#22929 = EDGE_LOOP ( 'NONE', ( #6772, #23263, #22814, #1939 ) ) ;
#22930 = ADVANCED_FACE ( 'NONE', ( #10767 ), #4017, .F. ) ;
#22931 = CARTESIAN_POINT ( 'NONE',  ( -4.197393957002303999, -7.773935952363655451E-14, -3.503767560748929810 ) ) ;
#22932 = APPLICATION_CONTEXT ( 'automotive_design' ) ;
#22933 = CIRCLE ( 'NONE', #20623, 20.00000000000000000 ) ;
#22934 = ORIENTED_EDGE ( 'NONE', *, *, #1512, .T. ) ;
#22935 = EDGE_CURVE ( 'NONE', #13307, #3094, #13069, .T. ) ;
#22936 = AXIS2_PLACEMENT_3D ( 'NONE', #10527, #12003, #2990 ) ;
#22937 = ORIENTED_EDGE ( 'NONE', *, *, #15455, .T. ) ;
#22938 = CARTESIAN_POINT ( 'NONE',  ( -24.19924082432261869, -6.487720809339531769, -144.9999999999999716 ) ) ;
#22939 = VERTEX_POINT ( 'NONE', #7718 ) ;
#22940 = B_SPLINE_CURVE_WITH_KNOTS ( 'NONE', 3,
 ( #20836, #9979, #15421, #10214, #2721, #551 ),
 .UNSPECIFIED., .F., .F.,
 ( 4, 2, 4 ),
 ( 0.004444412883774346255, 0.006655097293744437204, 0.008865781703714529019 ),
 .UNSPECIFIED. ) ;
#22941 = CARTESIAN_POINT ( 'NONE',  ( -35.00000000000001421, 90.00000000000001421, 3.000000000000001332 ) ) ;
#22942 = LINE ( 'NONE', #8478, #15658 ) ;
#22943 = EDGE_LOOP ( 'NONE', ( #9311, #6530, #11705, #21556 ) ) ;
#22944 = AXIS2_PLACEMENT_3D ( 'NONE', #20996, #9905, #9533 ) ;
#22945 = CARTESIAN_POINT ( 'NONE',  ( -280.2488155364689533, 269.9132285165672442, 145.5679143846943475 ) ) ;
#22946 = CARTESIAN_POINT ( 'NONE',  ( 146.0000000000001990, -801.0618695410406644, -27.94499999999356632 ) ) ;
#22947 = EDGE_LOOP ( 'NONE', ( #6925, #3940, #2368, #6885, #4568 ) ) ;
#22948 = UNCERTAINTY_MEASURE_WITH_UNIT (LENGTH_MEASURE( 1.000000000000000082E-05 ), #10972, 'distance_accuracy_value', 'NONE');
#22949 = CARTESIAN_POINT ( 'NONE',  ( -2.000000000000006661, 3.464101615137750834, 0.000000000000000000 ) ) ;
#22950 = PLANE ( 'NONE',  #8618 ) ;
#22951 = CARTESIAN_POINT ( 'NONE',  ( -137.9031948627971076, -44.80746418436799416, -90.00000000000000000 ) ) ;
#22952 = ADVANCED_FACE ( 'NONE', ( #14738 ), #22072, .T. ) ;
#22953 = AXIS2_PLACEMENT_3D ( 'NONE', #4155, #2217, #889 ) ;
#22954 = EDGE_CURVE ( 'NONE', #846, #8260, #19585, .T. ) ;
#22955 = DIRECTION ( 'NONE',  ( 0.000000000000000000, 0.000000000000000000, -1.000000000000000000 ) ) ;
#22956 = ORIENTED_EDGE ( 'NONE', *, *, #3237, .T. ) ;
#22957 = CARTESIAN_POINT ( 'NONE',  ( 100.0000000000000000, 269.9999999999999432, 145.0000000000000284 ) ) ;
#22958 = FILL_AREA_STYLE ('',( #6072 ) ) ;
#22959 = PRODUCT_DEFINITION_SHAPE ( 'NONE', 'NONE',  #23840 ) ;
#22961 = ORIENTED_EDGE ( 'NONE', *, *, #8714, .F. ) ;
#22960 = VERTEX_POINT ( 'NONE', #18566 ) ;
#22962 = DIRECTION ( 'NONE',  ( -6.982962677686266711E-15, 9.837870180509810443E-29, -1.000000000000000000 ) ) ;
#22963 = DIRECTION ( 'NONE',  ( 1.000000000000000000, -1.408839003528726857E-14, -6.982962677686266711E-15 ) ) ;
#22964 = AXIS2_PLACEMENT_3D ( 'NONE', #1741, #22036, #22147 ) ;
#22965 = CARTESIAN_POINT ( 'NONE',  ( -281.4928932188134354, -129.2000000000000455, -152.4000000000012847 ) ) ;
#22966 = DIRECTION ( 'NONE',  ( -0.000000000000000000, -0.000000000000000000, 1.000000000000000000 ) ) ;
#22967 = CARTESIAN_POINT ( 'NONE',  ( -282.2000000000000455, 268.0880230824754449, -146.3684665479254932 ) ) ;
#22968 = ORIENTED_EDGE ( 'NONE', *, *, #7230, .F. ) ;
#22969 = ADVANCED_FACE ( 'NONE', ( #17023 ), #4958, .T. ) ;
#22970 = DIRECTION ( 'NONE',  ( -0.000000000000000000, -0.000000000000000000, 1.000000000000000000 ) ) ;
#22971 = LINE ( 'NONE', #12523, #2654 ) ;
#22972 = CARTESIAN_POINT ( 'NONE',  ( 72.64999999999999147, -87.33333333333332860, 0.000000000000000000 ) ) ;
#22973 = ORIENTED_EDGE ( 'NONE', *, *, #14624, .F. ) ;
#22974 = DIRECTION ( 'NONE',  ( -3.469446951953614682E-16, 1.000000000000000000, -3.483493295888648978E-15 ) ) ;
#22975 = ORIENTED_EDGE ( 'NONE', *, *, #16136, .F. ) ;
#22976 = CARTESIAN_POINT ( 'NONE',  ( -282.2000000000012960, -74.99999999999899103, 90.00000000000000000 ) ) ;
#22977 = CYLINDRICAL_SURFACE ( 'NONE', #22953, 4.250000000000000000 ) ;
#22978 = EDGE_LOOP ( 'NONE', ( #16902, #5910, #2509, #20584, #1085, #13108, #7084, #19553, #20251, #4997, #16823, #11533, #4260, #13378, #18488, #5964, #10025, #23680, #10983, #23752, #16785, #10201, #12498, #23420, #21592, #10247, #923, #18531, #19056, #8508, #12065, #16338, #19468, #12113, #5811, #18882, #3877, #14363, #15703, #114, #4924, #16771, #18915, #14151, #23224, #8469, #7863, #17909, #7661 ) ) ;
#22979 = CIRCLE ( 'NONE', #1761, 20.30000000000000071 ) ;
#22980 = CARTESIAN_POINT ( 'NONE',  ( -285.2000000000014666, -127.0000000000000568, 146.4928932188134638 ) ) ;
#22981 = EDGE_LOOP ( 'NONE', ( #18543, #15557 ) ) ;
#22982 = DIRECTION ( 'NONE',  ( -0.000000000000000000, 1.000000000000000000, -3.469446951953613794E-15 ) ) ;
#22983 = CARTESIAN_POINT ( 'NONE',  ( -2.000000000000007550, -3.464101615137749945, 0.000000000000000000 ) ) ;
#22984 = DIRECTION ( 'NONE',  ( 0.000000000000000000, 1.000000000000000000, -1.103561164596346103E-15 ) ) ;
#22985 = CARTESIAN_POINT ( 'NONE',  ( 280.5724317483737309, 269.9290760626066117, 145.2497115627124629 ) ) ;
#22986 = CARTESIAN_POINT ( 'NONE',  ( -2.449848172108560540, -3.432307619358754724, -3.503702292528910078 ) ) ;
#22987 = LINE ( 'NONE', #8529, #13666 ) ;
#22988 = VERTEX_POINT ( 'NONE', #16883 ) ;
#22989 = EDGE_CURVE ( 'NONE', #22432, #12588, #347, .T. ) ;
#22990 =( NAMED_UNIT ( * ) SI_UNIT ( $, .STERADIAN. ) SOLID_ANGLE_UNIT ( ) );
#22991 = ADVANCED_FACE ( 'NONE', ( #9409 ), #13419, .T. ) ;
#22992 = DIRECTION ( 'NONE',  ( -1.000000000000000000, 0.000000000000000000, -6.982962677686266711E-15 ) ) ;
#22993 = CARTESIAN_POINT ( 'NONE',  ( 0.000000000000000000, -1000.000000000000000, -138.9999999999999716 ) ) ;
#22994 = ORIENTED_EDGE ( 'NONE', *, *, #6902, .F. ) ;
#22995 = SHAPE_REPRESENTATION ( 'hex flange nut gradea_iso_ISO - 4161 - M10 - N', ( #11210 ), #370 ) ;
#22996 = EDGE_LOOP ( 'NONE', ( #19925, #11259, #14931, #12728, #7479 ) ) ;
#22997 = FACE_OUTER_BOUND ( 'NONE', #3991, .T. ) ;
#22998 = DIRECTION ( 'NONE',  ( 1.110223024625157172E-14, 0.000000000000000000, -1.000000000000000000 ) ) ;
#22999 = AXIS2_PLACEMENT_3D ( 'NONE', #19712, #1822, #22106 ) ;
#23000 = EDGE_CURVE ( 'NONE', #21376, #21387, #11152, .T. ) ;
#23001 = ORIENTED_EDGE ( 'NONE', *, *, #13168, .F. ) ;
#23002 = CARTESIAN_POINT ( 'NONE',  ( -77.72886158240795851, -117.3074641843678876, -90.00000000000000000 ) ) ;
#23003 = EDGE_CURVE ( 'NONE', #11272, #17898, #4068, .T. ) ;
#23004 = CARTESIAN_POINT ( 'NONE',  ( 4.000000000000000000, -2.309401076758514915, -3.433295621305383349 ) ) ;
#23005 = CARTESIAN_POINT ( 'NONE',  ( -4.000000000000000000, 2.309401076758498483, -5.000000000000000000 ) ) ;
#23006 = LINE ( 'NONE', #22789, #11967 ) ;
#23007 = ORIENTED_EDGE ( 'NONE', *, *, #5849, .T. ) ;
#23008 = CARTESIAN_POINT ( 'NONE',  ( 34.99999999999999289, 90.00000000000000000, 3.000000000000001332 ) ) ;
#23009 = B_SPLINE_CURVE_WITH_KNOTS ( 'NONE', 3,
 ( #15132, #7861, #19192, #22931 ),
 .UNSPECIFIED., .F., .F.,
 ( 4, 4 ),
 ( 0.000000000000000000, 0.002452478801916376308 ),
 .UNSPECIFIED. ) ;
#23010 = CARTESIAN_POINT ( 'NONE',  ( -155.0000000000000284, -784.4690652294798383, -29.99999999999350564 ) ) ;
#23011 = CARTESIAN_POINT ( 'NONE',  ( 45.00000000000004974, -59.79999999999964189, 107.6500000000002331 ) ) ;
#23012 = ORIENTED_EDGE ( 'NONE', *, *, #13501, .F. ) ;
#23013 = CARTESIAN_POINT ( 'NONE',  ( 45.00000000000004974, -52.79999999999967031, 50.00000000000018474 ) ) ;
#23014 = CONTEXT_DEPENDENT_SHAPE_REPRESENTATION ( #15290, #14256 ) ;
#23015 = DIRECTION ( 'NONE',  ( 1.000000000000000000, 0.000000000000000000, 0.000000000000000000 ) ) ;
#23016 = CARTESIAN_POINT ( 'NONE',  ( -45.00000000000000000, 272.9999999999999432, -5.249999999999973355 ) ) ;
#23017 = AXIS2_PLACEMENT_3D ( 'NONE', #21000, #8445, #22807 ) ;
#23018 = CARTESIAN_POINT ( 'NONE',  ( -282.2000000000013529, -89.99999999999896261, -42.98333333333330586 ) ) ;
#23019 = DIRECTION ( 'NONE',  ( 0.000000000000000000, 0.000000000000000000, -1.000000000000000000 ) ) ;
#23020 = ORIENTED_EDGE ( 'NONE', *, *, #15687, .T. ) ;
#23021 = VERTEX_POINT ( 'NONE', #7581 ) ;
#23022 = CARTESIAN_POINT ( 'NONE',  ( -44.99999999999997868, -52.79999999999936477, 197.6500000000001478 ) ) ;
#23023 = CARTESIAN_POINT ( 'NONE',  ( 280.4357337430839721, 269.7771650631953548, 145.9755899421582512 ) ) ;
#23024 = ORIENTED_EDGE ( 'NONE', *, *, #1946, .F. ) ;
#23025 = EDGE_CURVE ( 'NONE', #10553, #6820, #18444, .T. ) ;
#23026 = ADVANCED_FACE ( 'NONE', ( #5790, #5656 ), #2258, .T. ) ;
#23027 = AXIS2_PLACEMENT_3D ( 'NONE', #10028, #9904, #17388 ) ;
#23028 = ORIENTED_EDGE ( 'NONE', *, *, #21837, .T. ) ;
#23029 = CARTESIAN_POINT ( 'NONE',  ( 0.000000000000000000, 1.865214261513747767E-15, 145.0000119999999697 ) ) ;
#23030 = EDGE_CURVE ( 'NONE', #2982, #13294, #9173, .T. ) ;
#23031 = CARTESIAN_POINT ( 'NONE',  ( -127.0272233253972587, 88.82062435171954462, 31.99235058689528444 ) ) ;
#23032 = ORIENTED_EDGE ( 'NONE', *, *, #8852, .F. ) ;
#23033 = EDGE_CURVE ( 'NONE', #23104, #22426, #20256, .T. ) ;
#23034 = CIRCLE ( 'NONE', #18034, 2.500000000000000444 ) ;
#23035 = CARTESIAN_POINT ( 'NONE',  ( -135.4738523116357953, -1075.311763300249822, -27.57873596473009314 ) ) ;
#23036 = VECTOR ( 'NONE', #21454, 1000.000000000000000 ) ;
#23037 = AXIS2_PLACEMENT_3D ( 'NONE', #11291, #16804, #18599 ) ;
#23038 = VERTEX_POINT ( 'NONE', #5537 ) ;
#23039 = ADVANCED_FACE ( 'NONE', ( #12950 ), #3711, .F. ) ;
#23040 = CARTESIAN_POINT ( 'NONE',  ( 30.00000000000000000, 0.000000000000000000, 2.054999999999993054 ) ) ;
#23041 = ADVANCED_FACE ( 'NONE', ( #12100 ), #15807, .F. ) ;
#23042 = FACE_OUTER_BOUND ( 'NONE', #15691, .T. ) ;
#23043 = EDGE_LOOP ( 'NONE', ( #22735, #20296 ) ) ;
#23044 = VERTEX_POINT ( 'NONE', #2390 ) ;
#23045 = CARTESIAN_POINT ( 'NONE',  ( -44.99999999999995026, -52.79999999999970584, 47.35000000000018616 ) ) ;
#23046 = CYLINDRICAL_SURFACE ( 'NONE', #17, 5.199999999999982414 ) ;
#23047 = CARTESIAN_POINT ( 'NONE',  ( 8.673617379884035472E-16, 4.618802153517012954, -5.000000000000000000 ) ) ;
#23048 = CIRCLE ( 'NONE', #7226, 145.0000000000000284 ) ;
#23049 = DIRECTION ( 'NONE',  ( -0.000000000000000000, -0.000000000000000000, 1.000000000000000000 ) ) ;
#23050 = ORIENTED_EDGE ( 'NONE', *, *, #15634, .T. ) ;
#23051 = VECTOR ( 'NONE', #16154, 999.9999999999998863 ) ;
#23052 = DIRECTION ( 'NONE',  ( 1.000000000000000000, 0.000000000000000000, 0.000000000000000000 ) ) ;
#23053 = AXIS2_PLACEMENT_3D ( 'NONE', #21088, #11962, #19273 ) ;
#23054 = SURFACE_SIDE_STYLE ('',( #2776 ) ) ;
#23055 = CONICAL_SURFACE ( 'NONE', #319, 2.041999999999999815, 1.047197551196591858 ) ;
#23056 = ORIENTED_EDGE ( 'NONE', *, *, #19479, .T. ) ;
#23057 = EDGE_CURVE ( 'NONE', #21068, #885, #22900, .T. ) ;
#23058 = ORIENTED_EDGE ( 'NONE', *, *, #17435, .T. ) ;
#23059 = CARTESIAN_POINT ( 'NONE',  ( -16.51654882469418695, -18.83872056949901008, -145.0000000000000000 ) ) ;
#23060 = VERTEX_POINT ( 'NONE', #2752 ) ;
#23061 = CARTESIAN_POINT ( 'NONE',  ( 0.000000000000000000, -2.357898499370431722, 2.818925648462311528E-15 ) ) ;
#23062 = DIRECTION ( 'NONE',  ( -0.5877852522924773560, 0.8090169943749444537, 0.000000000000000000 ) ) ;
#23063 = ORIENTED_EDGE ( 'NONE', *, *, #4292, .F. ) ;
#23064 = PRODUCT_DEFINITION_SHAPE ( 'NONE', 'NONE',  #5780 ) ;
#23065 = VECTOR ( 'NONE', #12096, 1000.000000000000000 ) ;
#23066 = EDGE_CURVE ( 'NONE', #3080, #10553, #17253, .T. ) ;
#23067 = VECTOR ( 'NONE', #1993, 1000.000000000000000 ) ;
#23068 = CARTESIAN_POINT ( 'NONE',  ( -280.1244266708878854, 269.9999999999999432, 145.2880230824751493 ) ) ;
#23069 = CARTESIAN_POINT ( 'NONE',  ( 0.000000000000000000, -2.342598717236900718, 4.057500000000001883 ) ) ;
#23070 = EDGE_CURVE ( 'NONE', #15682, #16958, #19394, .T. ) ;
#23071 = CIRCLE ( 'NONE', #16148, 1.500000000000001332 ) ;
#23072 = ORIENTED_EDGE ( 'NONE', *, *, #19625, .T. ) ;
#23073 = AXIS2_PLACEMENT_3D ( 'NONE', #1229, #7136, #12263 ) ;
#23074 = CARTESIAN_POINT ( 'NONE',  ( -4.211140560182196957, 2.431303136016537803, -3.745885042887433514 ) ) ;
#23075 = SURFACE_STYLE_USAGE ( .BOTH. , #4730 ) ;
#23076 = AXIS2_PLACEMENT_3D ( 'NONE', #21579, #17833, #4680 ) ;
#23077 = CARTESIAN_POINT ( 'NONE',  ( -4.613983237546153582, 6.452243898629808960, -7.591546097228401457 ) ) ;
#23078 = FACE_OUTER_BOUND ( 'NONE', #14802, .T. ) ;
#23079 = ORIENTED_EDGE ( 'NONE', *, *, #10634, .F. ) ;
#23080 = CARTESIAN_POINT ( 'NONE',  ( -175.1609685624542578, -1088.719770019218458, -29.99999999999322498 ) ) ;
#23082 = EDGE_LOOP ( 'NONE', ( #2516, #8766 ) ) ;
#23081 = EDGE_LOOP ( 'NONE', ( #19517, #2919, #23127, #7440 ) ) ;
#23083 = AXIS2_PLACEMENT_3D ( 'NONE', #9861, #13161, #9981 ) ;
#23084 = DIRECTION ( 'NONE',  ( -1.000000000000000000, 0.000000000000000000, -6.982962677686266711E-15 ) ) ;
#23086 = CIRCLE ( 'NONE', #2670, 145.0000000000000284 ) ;
#23085 = MECHANICAL_DESIGN_GEOMETRIC_PRESENTATION_REPRESENTATION (  '', ( #1113 ), #7284 ) ;
#23088 = LINE ( 'NONE', #6564, #22356 ) ;
#23087 = VECTOR ( 'NONE', #23128, 1000.000000000000000 ) ;
#23089 = CARTESIAN_POINT ( 'NONE',  ( 0.000000000000000000, -145.0000000000000284, 90.00000000000000000 ) ) ;
#23090 = VECTOR ( 'NONE', #19992, 1000.000000000000000 ) ;
#23091 = AXIS2_PLACEMENT_3D ( 'NONE', #5056, #19761, #2229 ) ;
#23092 = CIRCLE ( 'NONE', #18098, 1.500000000000001332 ) ;
#23093 = AXIS2_PLACEMENT_3D ( 'NONE', #13186, #3939, #11349 ) ;
#23094 = FACE_OUTER_BOUND ( 'NONE', #14264, .T. ) ;
#23095 = CARTESIAN_POINT ( 'NONE',  ( 2.500000000000002220, -1.178949249685218970, -2.041999999999998483 ) ) ;
#23096 = CARTESIAN_POINT ( 'NONE',  ( -280.6807971656549512, 272.9999999999999432, -145.1244294735508618 ) ) ;
#23097 = EDGE_LOOP ( 'NONE', ( #11689, #17105 ) ) ;
#23098 = CARTESIAN_POINT ( 'NONE',  ( -20.00000000000000000, -1000.000000000000000, 138.9999999999999716 ) ) ;
#23099 = AXIS2_PLACEMENT_3D ( 'NONE', #405, #18370, #22230 ) ;
#23100 = CARTESIAN_POINT ( 'NONE',  ( 99.99999999999997158, 34.99999999999995026, 150.2000000000010971 ) ) ;
#23101 = CARTESIAN_POINT ( 'NONE',  ( 0.000000000000000000, 0.000000000000000000, -150.0000000000000000 ) ) ;
#23102 = ORIENTED_EDGE ( 'NONE', *, *, #17663, .T. ) ;
#23103 = CARTESIAN_POINT ( 'NONE',  ( -2.742827927723112236, -3.035229711105190464, -3.433252694550595230 ) ) ;
#23104 = VERTEX_POINT ( 'NONE', #697 ) ;
#23105 = PLANE ( 'NONE',  #6935 ) ;
#23106 = DIRECTION ( 'NONE',  ( 0.000000000000000000, 0.000000000000000000, -1.000000000000000000 ) ) ;
#23108 = VECTOR ( 'NONE', #19359, 1000.000000000000000 ) ;
#23107 = AXIS2_PLACEMENT_3D ( 'NONE', #21046, #8016, #4506 ) ;
#23109 = ORIENTED_EDGE ( 'NONE', *, *, #7800, .T. ) ;
#23110 = CIRCLE ( 'NONE', #18864, 20.00000000000000000 ) ;
#23111 = CARTESIAN_POINT ( 'NONE',  ( 40.00000000000000000, 100.0000000000000000, 145.0000000000000000 ) ) ;
#23112 = AXIS2_PLACEMENT_3D ( 'NONE', #2477, #21074, #17222 ) ;
#23113 = VECTOR ( 'NONE', #878, 1000.000000000000000 ) ;
#23114 = LINE ( 'NONE', #11938, #10023 ) ;
#23115 = VECTOR ( 'NONE', #5494, 1000.000000000000000 ) ;
#23116 = VECTOR ( 'NONE', #1541, 1000.000000000000000 ) ;
#23117 = LINE ( 'NONE', #3070, #2230 ) ;
#23118 = DIRECTION ( 'NONE',  ( -1.000000000000000000, 0.000000000000000000, 0.000000000000000000 ) ) ;
#23119 = DIRECTION ( 'NONE',  ( -4.862939117679700002E-15, 5.011346215908450209E-15, 1.000000000000000000 ) ) ;
#23120 = DIRECTION ( 'NONE',  ( 0.000000000000000000, 0.000000000000000000, 1.000000000000000000 ) ) ;
#23121 = DIRECTION ( 'NONE',  ( 0.000000000000000000, 1.000000000000000000, -5.286776307738891306E-15 ) ) ;
#23122 = VERTEX_POINT ( 'NONE', #23018 ) ;
#23123 = FILL_AREA_STYLE ('',( #8395 ) ) ;
#23124 = CARTESIAN_POINT ( 'NONE',  ( 145.0000000000000284, -500.0000000000000000, 27.50000000000001066 ) ) ;
#23125 = LINE ( 'NONE', #8181, #17384 ) ;
#23126 = EDGE_LOOP ( 'NONE', ( #23707, #20576, #20084, #7704 ) ) ;
#23127 = ORIENTED_EDGE ( 'NONE', *, *, #11514, .T. ) ;
#23128 = DIRECTION ( 'NONE',  ( -1.000000000000000000, -0.000000000000000000, -0.000000000000000000 ) ) ;
#23129 = DIRECTION ( 'NONE',  ( -1.000000000000000000, 0.000000000000000000, 0.000000000000000000 ) ) ;
#23130 = AXIS2_PLACEMENT_3D ( 'NONE', #4063, #9770, #583 ) ;
#23131 = MECHANICAL_DESIGN_GEOMETRIC_PRESENTATION_REPRESENTATION (  '', ( #19268 ), #4242 ) ;
#23132 = AXIS2_PLACEMENT_3D ( 'NONE', #19771, #10630, #7987 ) ;
#23133 = CIRCLE ( 'NONE', #2698, 2.649999999999985700 ) ;
#23134 = PLANE ( 'NONE',  #23703 ) ;
#23135 = AXIS2_PLACEMENT_3D ( 'NONE', #12657, #3431, #19972 ) ;
#23136 = CARTESIAN_POINT ( 'NONE',  ( 131.5594662024482489, 81.95796442704008200, 30.65375098132849985 ) ) ;
#23137 = DIRECTION ( 'NONE',  ( 0.000000000000000000, 0.000000000000000000, -1.000000000000000000 ) ) ;
#23138 = AXIS2_PLACEMENT_3D ( 'NONE', #22298, #3942, #11352 ) ;
#23139 = DIRECTION ( 'NONE',  ( 0.9289202219288174023, 0.3702799228849934510, 6.982962677686266711E-15 ) ) ;
#23140 = VERTEX_POINT ( 'NONE', #17128 ) ;
#23141 = EDGE_CURVE ( 'NONE', #22099, #13958, #13116, .T. ) ;
#23142 = DIRECTION ( 'NONE',  ( 1.000000000000000000, -0.000000000000000000, -0.000000000000000000 ) ) ;
#23143 = LINE ( 'NONE', #16378, #4639 ) ;
#23144 = EDGE_CURVE ( 'NONE', #8155, #12774, #21170, .T. ) ;
#23145 = LINE ( 'NONE', #17246, #16369 ) ;
#23146 = EDGE_CURVE ( 'NONE', #1216, #17208, #13781, .T. ) ;
#23147 = ORIENTED_EDGE ( 'NONE', *, *, #9299, .T. ) ;
#23148 = CARTESIAN_POINT ( 'NONE',  ( -129.2206655591605511, -1072.408698320350595, 32.05500000000640171 ) ) ;
#23149 = DIRECTION ( 'NONE',  ( -0.000000000000000000, -1.000000000000000000, -0.000000000000000000 ) ) ;
#23150 = CARTESIAN_POINT ( 'NONE',  ( 65.00000000000001421, -52.79999999999938609, 125.0000000000002274 ) ) ;
#23151 = CARTESIAN_POINT ( 'NONE',  ( 1.641270926519074358, -1025.000000000000000, -145.0000000000001421 ) ) ;
#23152 = AXIS2_PLACEMENT_3D ( 'NONE', #8696, #1567, #12362 ) ;
#23153 = LINE ( 'NONE', #3105, #19205 ) ;
#23154 = EDGE_CURVE ( 'NONE', #12421, #15087, #20786, .T. ) ;
#23155 = CARTESIAN_POINT ( 'NONE',  ( -44.99999999999995026, -52.79999999999967741, 105.0000000000001990 ) ) ;
#23156 = LINE ( 'NONE', #11980, #22840 ) ;
#23157 = VECTOR ( 'NONE', #21623, 1000.000000000000000 ) ;
#23158 = AXIS2_PLACEMENT_3D ( 'NONE', #23211, #13843, #17320 ) ;
#23159 = ORIENTED_EDGE ( 'NONE', *, *, #12004, .F. ) ;
#23160 = EDGE_LOOP ( 'NONE', ( #5938, #17850, #1668, #665 ) ) ;
#23161 = DIRECTION ( 'NONE',  ( 0.000000000000000000, -2.618450529776326854E-15, -1.000000000000000000 ) ) ;
#23162 = CARTESIAN_POINT ( 'NONE',  ( 280.6839617489739567, 269.4578961534455743, 146.4533442688711204 ) ) ;
#23163 = ORIENTED_EDGE ( 'NONE', *, *, #13645, .F. ) ;
#23164 = CARTESIAN_POINT ( 'NONE',  ( -9.999999999999998224, 0.000000000000000000, 150.0000000000000284 ) ) ;
#23165 = VERTEX_POINT ( 'NONE', #2852 ) ;
#23166 = CARTESIAN_POINT ( 'NONE',  ( -281.4928932188135491, 267.7999999999999545, 145.0000000000000284 ) ) ;
#23167 = CARTESIAN_POINT ( 'NONE',  ( -126.4950807468203919, 89.57684269074565009, 29.33965772977898823 ) ) ;
#23168 = ORIENTED_EDGE ( 'NONE', *, *, #6633, .T. ) ;
#23169 = LINE ( 'NONE', #14029, #2112 ) ;
#23170 = ORIENTED_EDGE ( 'NONE', *, *, #2196, .T. ) ;
#23171 = CARTESIAN_POINT ( 'NONE',  ( -287.4000000000014552, -132.2000000000000455, -146.4928932188134070 ) ) ;
#23172 = CYLINDRICAL_SURFACE ( 'NONE', #15196, 2.500000000000000444 ) ;
#23173 = VERTEX_POINT ( 'NONE', #15331 ) ;
#23174 = ORIENTED_EDGE ( 'NONE', *, *, #60, .T. ) ;
#23175 = LINE ( 'NONE', #6755, #17726 ) ;
#23176 = PRODUCT_DEFINITION_SHAPE ( 'NONE', 'NONE',  #23875 ) ;
#23177 = ADVANCED_FACE ( 'NONE', ( #18927 ), #17593, .F. ) ;
#23178 = DIRECTION ( 'NONE',  ( 1.000000000000000000, -3.495664435217746987E-15, 0.000000000000000000 ) ) ;
#23179 = CARTESIAN_POINT ( 'NONE',  ( 3.455068668934414777, -2.624017327439094327, -3.316620875263732504 ) ) ;
#23180 = EDGE_CURVE ( 'NONE', #15388, #18827, #11979, .T. ) ;
#23181 = LINE ( 'NONE', #13246, #3006 ) ;
#23182 = CARTESIAN_POINT ( 'NONE',  ( -281.4928932188134922, -129.2000000000000455, -177.2000000000013529 ) ) ;
#23183 = EDGE_CURVE ( 'NONE', #10816, #8336, #8201, .T. ) ;
#23184 = ORIENTED_EDGE ( 'NONE', *, *, #10844, .T. ) ;
#23185 = LINE ( 'NONE', #6764, #19532 ) ;
#23186 =( NAMED_UNIT ( * ) PLANE_ANGLE_UNIT ( ) SI_UNIT ( $, .RADIAN. ) );
#23187 = ADVANCED_FACE ( 'NONE', ( #22667 ), #21102, .T. ) ;
#23188 = ORIENTED_EDGE ( 'NONE', *, *, #10132, .F. ) ;
#23189 = EDGE_CURVE ( 'NONE', #9666, #14205, #8838, .T. ) ;
#23190 = VERTEX_POINT ( 'NONE', #21234 ) ;
#23191 = CARTESIAN_POINT ( 'NONE',  ( -12.52400585386708443, -21.69891193169445032, -145.0000000000000000 ) ) ;
#23192 = ORIENTED_EDGE ( 'NONE', *, *, #18551, .F. ) ;
#23193 = FACE_OUTER_BOUND ( 'NONE', #15757, .T. ) ;
#23194 = DIRECTION ( 'NONE',  ( 0.000000000000000000, -0.4999999999999992228, 0.8660254037844390407 ) ) ;
#23195 = EDGE_LOOP ( 'NONE', ( #3690, #3121, #23647, #4363, #8755 ) ) ;
#23196 = CARTESIAN_POINT ( 'NONE',  ( 5.000000000000000888, 0.000000000000000000, -10.00000000000000000 ) ) ;
#23197 = FACE_OUTER_BOUND ( 'NONE', #2437, .T. ) ;
#23198 = EDGE_LOOP ( 'NONE', ( #11666, #7832, #23518, #14885 ) ) ;
#23199 = PLANE ( 'NONE',  #17760 ) ;
#23200 = CARTESIAN_POINT ( 'NONE',  ( 5.000000000000000000, -4.685197434473811207, 4.770489558936219510E-15 ) ) ;
#23201 = DIRECTION ( 'NONE',  ( -0.9423651898111408132, -0.3345860861306287348, 6.982962677686266711E-15 ) ) ;
#23202 = DIRECTION ( 'NONE',  ( 1.000000000000000000, 0.000000000000000000, 0.000000000000000000 ) ) ;
#23203 = ORIENTED_EDGE ( 'NONE', *, *, #10568, .F. ) ;
#23204 = DIRECTION ( 'NONE',  ( 1.000000000000000000, 0.000000000000000000, 0.000000000000000000 ) ) ;
#23206 = ORIENTED_EDGE ( 'NONE', *, *, #5579, .F. ) ;
#23205 = EDGE_LOOP ( 'NONE', ( #15762, #15312, #1878, #22150, #15776, #18705 ) ) ;
#23207 = DIRECTION ( 'NONE',  ( 1.000000000000000000, 0.000000000000000000, 0.000000000000000000 ) ) ;
#23208 = EDGE_CURVE ( 'NONE', #22764, #16743, #13887, .T. ) ;
#23209 = EDGE_CURVE ( 'NONE', #3131, #15388, #14263, .T. ) ;
#23210 = CARTESIAN_POINT ( 'NONE',  ( 7.500000000000000000, 3.160172554975063886, -7.231829826456836585 ) ) ;
#23211 = CARTESIAN_POINT ( 'NONE',  ( 45.00000000000000000, 272.9999999999999432, 0.000000000000000000 ) ) ;
#23212 = EDGE_CURVE ( 'NONE', #3595, #13252, #7265, .T. ) ;
#23213 = FACE_OUTER_BOUND ( 'NONE', #17289, .T. ) ;
#23214 = LINE ( 'NONE', #19346, #14658 ) ;
#23215 = CARTESIAN_POINT ( 'NONE',  ( -282.1132285165673466, 268.3679143846943020, -146.2440776823445390 ) ) ;
#23216 = ORIENTED_EDGE ( 'NONE', *, *, #23711, .F. ) ;
#23217 = CARTESIAN_POINT ( 'NONE',  ( 7.499999999999999112, -2.930060224340428565, -0.4701183149080248036 ) ) ;
#23218 = ORIENTED_EDGE ( 'NONE', *, *, #18935, .F. ) ;
#23219 = DIRECTION ( 'NONE',  ( -1.000000000000000000, 3.495664435217746987E-15, 0.000000000000000000 ) ) ;
#23220 = SURFACE_STYLE_USAGE ( .BOTH. , #12061 ) ;
#23221 = ORIENTED_EDGE ( 'NONE', *, *, #19934, .T. ) ;
#23222 = AXIS2_PLACEMENT_3D ( 'NONE', #16329, #23790, #2045 ) ;
#23223 = CARTESIAN_POINT ( 'NONE',  ( -90.00000000000000000, -74.99999999999998579, 3.000000000000002665 ) ) ;
#23224 = ORIENTED_EDGE ( 'NONE', *, *, #6770, .T. ) ;
#23225 = DIRECTION ( 'NONE',  ( 1.000000000000000000, 0.000000000000000000, 0.000000000000000000 ) ) ;
#23226 = DIRECTION ( 'NONE',  ( 1.000000000000000000, 0.000000000000000000, 0.000000000000000000 ) ) ;
#23227 = VERTEX_POINT ( 'NONE', #15574 ) ;
#23228 = CARTESIAN_POINT ( 'NONE',  ( -194.7500000000005116, -784.4690652294792699, -32.49999999999322853 ) ) ;
#23229 = CARTESIAN_POINT ( 'NONE',  ( -137.9031948627971076, -44.80746418436799416, -90.00000000000000000 ) ) ;
#23230 = FACE_OUTER_BOUND ( 'NONE', #2584, .T. ) ;
#23231 = CARTESIAN_POINT ( 'NONE',  ( 0.000000000000000000, 2.357898499370432166, -2.385244779468109755E-15 ) ) ;
#23232 = CARTESIAN_POINT ( 'NONE',  ( 282.1999999999998181, 268.0905802150184627, 146.3673618604587432 ) ) ;
#23233 = DIRECTION ( 'NONE',  ( -1.000000000000000000, 0.000000000000000000, 0.000000000000000000 ) ) ;
#23234 = FACE_OUTER_BOUND ( 'NONE', #22996, .T. ) ;
#23235 = EDGE_LOOP ( 'NONE', ( #1448, #20388, #16230, #21748 ) ) ;
#23236 =( LENGTH_UNIT ( ) NAMED_UNIT ( * ) SI_UNIT ( .MILLI., .METRE. ) );
#23237 = FACE_OUTER_BOUND ( 'NONE', #16018, .T. ) ;
#23238 = DIRECTION ( 'NONE',  ( 0.000000000000000000, 1.000000000000000000, 0.000000000000000000 ) ) ;
#23239 = ORIENTED_EDGE ( 'NONE', *, *, #15235, .T. ) ;
#23240 = VECTOR ( 'NONE', #12842, 1000.000000000000000 ) ;
#23241 = ORIENTED_EDGE ( 'NONE', *, *, #23704, .T. ) ;
#23242 = CARTESIAN_POINT ( 'NONE',  ( 5.200000000000002842, 0.000000000000000000, -2.700000000000000622 ) ) ;
#23243 = DIRECTION ( 'NONE',  ( 1.000000000000000000, 0.000000000000000000, 0.000000000000000000 ) ) ;
#23244 = DIRECTION ( 'NONE',  ( 1.000000000000000000, -3.495664435217746987E-15, -0.000000000000000000 ) ) ;
#23245 = LINE ( 'NONE', #13769, #5720 ) ;
#23246 = CARTESIAN_POINT ( 'NONE',  ( 65.00000000000004263, -56.79999999999959925, 65.00000000000019895 ) ) ;
#23247 = CARTESIAN_POINT ( 'NONE',  ( 2.500000000000002220, 2.357898499370434386, -3.469446951953614189E-15 ) ) ;
#23248 = ORIENTED_EDGE ( 'NONE', *, *, #9923, .F. ) ;
#23249 = DIRECTION ( 'NONE',  ( 0.000000000000000000, -1.177509268541832635E-16, 1.000000000000000000 ) ) ;
#23250 = PLANE ( 'NONE',  #5798 ) ;
#23251 = VECTOR ( 'NONE', #3064, 1000.000000000000000 ) ;
#23252 = ORIENTED_EDGE ( 'NONE', *, *, #22989, .T. ) ;
#23253 = DIRECTION ( 'NONE',  ( -4.625929269271485914E-16, -3.469446951953614583E-15, -1.000000000000000000 ) ) ;
#23254 = CIRCLE ( 'NONE', #20544, 2.500000000000002220 ) ;
#23255 = APPLICATION_CONTEXT ( 'automotive_design' ) ;
#23256 = DIRECTION ( 'NONE',  ( 0.000000000000000000, 0.4999999999999991118, -0.8660254037844391517 ) ) ;
#23257 = DIRECTION ( 'NONE',  ( 1.000000000000000000, -0.000000000000000000, -0.000000000000000000 ) ) ;
#23258 = CARTESIAN_POINT ( 'NONE',  ( 18.83872056894873381, -1016.516548825274981, -145.0000000000001421 ) ) ;
#23259 = DIRECTION ( 'NONE',  ( 0.000000000000000000, 1.000000000000000000, -1.224646799147353207E-16 ) ) ;
#23260 = FACE_OUTER_BOUND ( 'NONE', #22826, .T. ) ;
#23261 = ADVANCED_FACE ( 'NONE', ( #18080 ), #5157, .F. ) ;
#23262 = CARTESIAN_POINT ( 'NONE',  ( 0.000000000000000000, 0.000000000000000000, 0.000000000000000000 ) ) ;
#23263 = ORIENTED_EDGE ( 'NONE', *, *, #4062, .F. ) ;
#23264 = EDGE_LOOP ( 'NONE', ( #7739, #16918, #674, #22844 ) ) ;
#23265 = CARTESIAN_POINT ( 'NONE',  ( -2.699999999999997513, 2.449293598294706119E-15, 19.99999999999999645 ) ) ;
#23266 = CARTESIAN_POINT ( 'NONE',  ( 2.500000000000002220, -2.357898499370430834, 3.469446951953614189E-15 ) ) ;
#23267 = ORIENTED_EDGE ( 'NONE', *, *, #3710, .T. ) ;
#23268 = VECTOR ( 'NONE', #12358, 1000.000000000000000 ) ;
#23269 = PRODUCT ( 'angular contact ball bearing_68_iso_ISO 15 ABB - 1740 - 38,SI,NC,38_68', 'angular contact ball bearing_68_iso_ISO 15 ABB - 1740 - 38,SI,NC,38_68', '', ( #14736 ) ) ;
#23270 = ADVANCED_FACE ( 'NONE', ( #3460 ), #19643, .F. ) ;
#23272 = B_SPLINE_CURVE_WITH_KNOTS ( 'NONE', 3,
 ( #8799, #6985, #21107, #15692, #6624, #14019, #21346, #13911, #10382, #19398, #19519, #2975, #1186, #8561, #15928, #4926 ),
 .UNSPECIFIED., .F., .F.,
 ( 4, 2, 2, 2, 2, 2, 2, 4 ),
 ( 0.000000000000000000, 0.0009361184303671104363, 0.001404177645550636760, 0.001872236860734162976, 0.002340296075917688758, 0.002808355291101215408, 0.003276414506284741190, 0.003744473721468266972 ),
 .UNSPECIFIED. ) ;
#23271 = DIRECTION ( 'NONE',  ( 1.000000000000000000, 0.000000000000000000, 0.000000000000000000 ) ) ;
#23274 = AXIS2_PLACEMENT_3D ( 'NONE', #14174, #10301, #15865 ) ;
#23273 = DIRECTION ( 'NONE',  ( -1.000000000000000000, 0.000000000000000000, -0.000000000000000000 ) ) ;
#23275 = EDGE_CURVE ( 'NONE', #7513, #3739, #23736, .T. ) ;
#23276 = ORIENTED_EDGE ( 'NONE', *, *, #13674, .T. ) ;
#23277 = DIRECTION ( 'NONE',  ( 0.000000000000000000, -1.000000000000000000, 0.000000000000000000 ) ) ;
#23278 = CARTESIAN_POINT ( 'NONE',  ( -35.00000000000001421, 90.00000000000001421, 3.000000000000000000 ) ) ;
#23279 = ORIENTED_EDGE ( 'NONE', *, *, #3943, .F. ) ;
#23280 = CARTESIAN_POINT ( 'NONE',  ( -146.0000000000005116, -204.4690652294800657, -29.99999999999356604 ) ) ;
#23281 = ADVANCED_FACE ( 'NONE', ( #10872, #21458, #6980 ), #14013, .T. ) ;
#23282 = ORIENTED_EDGE ( 'NONE', *, *, #21677, .F. ) ;
#23283 = CARTESIAN_POINT ( 'NONE',  ( 2.500000000000000000, -1.178949249685213863, 2.042000000000002924 ) ) ;
#23284 = CARTESIAN_POINT ( 'NONE',  ( -7.894787914004607998, -0.7661396099416333261, -7.591390474663429089 ) ) ;
#23285 = ORIENTED_EDGE ( 'NONE', *, *, #18895, .F. ) ;
#23286 = ORIENTED_EDGE ( 'NONE', *, *, #21402, .F. ) ;
#23287 = CARTESIAN_POINT ( 'NONE',  ( 134.1180124237195912, 77.70044921554776352, -29.67081494451416646 ) ) ;
#23288 = PRESENTATION_LAYER_ASSIGNMENT (  '', '', ( #20193 ) ) ;
#23289 = CARTESIAN_POINT ( 'NONE',  ( -277.2000000000010118, -19.99999999999903011, 105.0000000000000000 ) ) ;
#23290 = CARTESIAN_POINT ( 'NONE',  ( 0.000000000000000000, 0.000000000000000000, -9.974600000000000577 ) ) ;
#23291 = VECTOR ( 'NONE', #5397, 1000.000000000000000 ) ;
#23292 = DIRECTION ( 'NONE',  ( -3.051161311199799893E-31, -1.000000000000000000, 0.000000000000000000 ) ) ;
#23293 = VECTOR ( 'NONE', #17492, 1000.000000000000000 ) ;
#23294 = DIRECTION ( 'NONE',  ( -0.7232617928448825673, 0.6905739489807055653, 6.982962677686266711E-15 ) ) ;
#23295 = ORIENTED_EDGE ( 'NONE', *, *, #12194, .T. ) ;
#23296 = CARTESIAN_POINT ( 'NONE',  ( 25.00000000000001421, -37.41657386773940885, 155.0000000000001990 ) ) ;
#23297 =( NAMED_UNIT ( * ) SI_UNIT ( $, .STERADIAN. ) SOLID_ANGLE_UNIT ( ) );
#23298 = ORIENTED_EDGE ( 'NONE', *, *, #22436, .F. ) ;
#23299 = EDGE_CURVE ( 'NONE', #9980, #20480, #12570, .T. ) ;
#23300 = ADVANCED_FACE ( 'NONE', ( #23389, #23625 ), #23516, .F. ) ;
#23301 = VERTEX_POINT ( 'NONE', #7082 ) ;
#23302 = CIRCLE ( 'NONE', #12946, 2.499999999999998668 ) ;
#23303 = CARTESIAN_POINT ( 'NONE',  ( 30.00000000000000000, 2.789133085058097101E-16, -2.055000000000006821 ) ) ;
#23304 = AXIS2_PLACEMENT_3D ( 'NONE', #12295, #19602, #58 ) ;
#23305 = EDGE_LOOP ( 'NONE', ( #8596, #6271, #2679, #17743 ) ) ;
#23306 = CARTESIAN_POINT ( 'NONE',  ( 3.093533885183100018, 6.874201416487501604, -7.446478553995813598 ) ) ;
#23307 = ADVANCED_FACE ( 'NONE', ( #4799 ), #12461, .T. ) ;
#23308 = ADVANCED_FACE ( 'NONE', ( #23260 ), #18196, .F. ) ;
#23309 = VERTEX_POINT ( 'NONE', #1180 ) ;
#23310 = CARTESIAN_POINT ( 'NONE',  ( -136.3242110351073109, -1073.761323382753744, 32.24990070396070507 ) ) ;
#23311 = DIRECTION ( 'NONE',  ( -1.000000000000000000, 1.408839003528726857E-14, 6.982962677686266711E-15 ) ) ;
#23312 = VERTEX_POINT ( 'NONE', #1644 ) ;
#23313 = ADVANCED_FACE ( 'NONE', ( #5274 ), #8794, .T. ) ;
#23314 = PRODUCT_RELATED_PRODUCT_CATEGORY ( 'part', '', ( #23666 ) ) ;
#23315 = DIRECTION ( 'NONE',  ( -1.110223024625157172E-14, 0.000000000000000000, -1.000000000000000000 ) ) ;
#23316 = CARTESIAN_POINT ( 'NONE',  ( -280.6842353883612304, 269.4574776399286975, 146.4538215477170127 ) ) ;
#23317 = EDGE_CURVE ( 'NONE', #18096, #22988, #11172, .T. ) ;
#23318 = CARTESIAN_POINT ( 'NONE',  ( -7.264118654998712010, 4.945491722146218905, -7.907633014911216840 ) ) ;
#23319 = CARTESIAN_POINT ( 'NONE',  ( 124.6651547408753800, -1092.106598813447590, -27.51562286569270199 ) ) ;
#23320 = VECTOR ( 'NONE', #7101, 1000.000000000000000 ) ;
#23321 = CARTESIAN_POINT ( 'NONE',  ( -7.500000000000000000, -2.571118828324945760, -0.3627527587569098766 ) ) ;
#23322 = EDGE_LOOP ( 'NONE', ( #13744, #18969 ) ) ;
#23323 = CYLINDRICAL_SURFACE ( 'NONE', #2263, 5.249999999999942268 ) ;
#23324 =( NAMED_UNIT ( * ) SI_UNIT ( $, .STERADIAN. ) SOLID_ANGLE_UNIT ( ) );
#23326 = ORIENTED_EDGE ( 'NONE', *, *, #13896, .F. ) ;
#23325 = ORIENTED_EDGE ( 'NONE', *, *, #23299, .T. ) ;
#23327 = VECTOR ( 'NONE', #16543, 1000.000000000000000 ) ;
#23328 = DIRECTION ( 'NONE',  ( 2.832769448823989808E-16, -1.000000000000000000, 3.469446951953613794E-15 ) ) ;
#23329 = CARTESIAN_POINT ( 'NONE',  ( -6.874999999999995559, 4.690970937165706900, -7.298562697733101068 ) ) ;
#23330 = CARTESIAN_POINT ( 'NONE',  ( 100.0000000000000000, 250.0000000000000000, -124.9999999999999716 ) ) ;
#23331 = FACE_OUTER_BOUND ( 'NONE', #17948, .T. ) ;
#23332 = CARTESIAN_POINT ( 'NONE',  ( -280.5758453455904942, 269.9427398886703031, -145.2488155364688396 ) ) ;
#23333 = ADVANCED_FACE ( 'NONE', ( #12683 ), #16155, .F. ) ;
#23334 = CONICAL_SURFACE ( 'NONE', #22172, 2.055000000000001492, 0.7853981633974633780 ) ;
#23335 = EDGE_LOOP ( 'NONE', ( #5934, #23727, #17460, #14660 ) ) ;
#23336 = FACE_OUTER_BOUND ( 'NONE', #20171, .T. ) ;
#23337 = ORIENTED_EDGE ( 'NONE', *, *, #9723, .T. ) ;
#23338 = ADVANCED_FACE ( 'NONE', ( #10378 ), #16039, .F. ) ;
#23339 = DIRECTION ( 'NONE',  ( -0.000000000000000000, -0.000000000000000000, 1.000000000000000000 ) ) ;
#23340 = CARTESIAN_POINT ( 'NONE',  ( -7.499999999999999112, 41.99999999999998579, 100.0000000000000000 ) ) ;
#23341 = ORIENTED_EDGE ( 'NONE', *, *, #19584, .F. ) ;
#23342 = CIRCLE ( 'NONE', #5219, 2.500000000000002220 ) ;
#23343 = CARTESIAN_POINT ( 'NONE',  ( 99.99999999999987210, -129.2000000000000455, 7.690461757479017101E-15 ) ) ;
#23344 = EDGE_LOOP ( 'NONE', ( #11048, #3635, #8877, #23792, #11649 ) ) ;
#23345 = AXIS2_PLACEMENT_3D ( 'NONE', #7959, #4209, #16776 ) ;
#23346 = CARTESIAN_POINT ( 'NONE',  ( -129.6400180686265173, -1072.557589128678728, 30.00000000000641975 ) ) ;
#23347 = DIRECTION ( 'NONE',  ( -1.000000000000000000, 0.000000000000000000, 0.000000000000000000 ) ) ;
#23348 = ADVANCED_FACE ( 'NONE', ( #17843 ), #14249, .F. ) ;
#23349 = VERTEX_POINT ( 'NONE', #16993 ) ;
#23350 = EDGE_CURVE ( 'NONE', #5262, #5300, #6125, .T. ) ;
#23351 = PRESENTATION_STYLE_ASSIGNMENT (( #21775 ) ) ;
#23352 = FILL_AREA_STYLE_COLOUR ( '', #23471 ) ;
#23353 = CARTESIAN_POINT ( 'NONE',  ( 0.000000000000000000, 2.755455298081544778E-15, -22.50000000000000000 ) ) ;
#23354 = CARTESIAN_POINT ( 'NONE',  ( 3.678949249685231848, 0.000000000000000000, 0.000000000000000000 ) ) ;
#23355 = CARTESIAN_POINT ( 'NONE',  ( 121.0905917848626814, -1085.936264790783525, 30.00000000000641620 ) ) ;
#23356 = AXIS2_PLACEMENT_3D ( 'NONE', #23508, #16270, #7072 ) ;
#23357 = CARTESIAN_POINT ( 'NONE',  ( -105.0000000000000000, -29.99999999999998579, 0.000000000000000000 ) ) ;
#23358 = LINE ( 'NONE', #4531, #14801 ) ;
#23359 = ORIENTED_EDGE ( 'NONE', *, *, #13016, .F. ) ;
#23360 = AXIS2_PLACEMENT_3D ( 'NONE', #21740, #122, #5202 ) ;
#23361 = FILL_AREA_STYLE_COLOUR ( '', #20780 ) ;
#23362 = CARTESIAN_POINT ( 'NONE',  ( -285.2000000000008981, 30.00000000000101963, -105.0000000000000142 ) ) ;
#23363 = CARTESIAN_POINT ( 'NONE',  ( -4.211405944401398038, -2.460460786169389902, -3.751298493805494072 ) ) ;
#23364 = ORIENTED_EDGE ( 'NONE', *, *, #23478, .F. ) ;
#23365 = VERTEX_POINT ( 'NONE', #13167 ) ;
#23366 = FACE_OUTER_BOUND ( 'NONE', #16319, .T. ) ;
#23367 = LINE ( 'NONE', #6826, #9991 ) ;
#23369 = CARTESIAN_POINT ( 'NONE',  ( 80.00000000000000000, -62.00000000000001421, 5.199999999999997513 ) ) ;
#23368 = PRODUCT_DEFINITION_SHAPE ( 'NONE', 'NONE',  #23837 ) ;
#23370 = EDGE_CURVE ( 'NONE', #19782, #3909, #9142, .T. ) ;
#23371 = CIRCLE ( 'NONE', #13007, 24.99999999999998224 ) ;
#23372 = CARTESIAN_POINT ( 'NONE',  ( 132.8404720734530144, 79.86494211668951948, 32.50000000000646594 ) ) ;
#23373 = CARTESIAN_POINT ( 'NONE',  ( -282.6054396500289840, 272.3132312761073308, -145.4975000228326394 ) ) ;
#23374 = ORIENTED_EDGE ( 'NONE', *, *, #18278, .T. ) ;
#23375 = DIRECTION ( 'NONE',  ( 0.000000000000000000, 0.000000000000000000, -1.000000000000000000 ) ) ;
#23376 = EDGE_LOOP ( 'NONE', ( #22828, #17881, #8927, #13784 ) ) ;
#23377 = CYLINDRICAL_SURFACE ( 'NONE', #19891, 2.649999999999985700 ) ;
#23378 = DIRECTION ( 'NONE',  ( -0.000000000000000000, 0.4999999999999979461, -0.8660254037844397068 ) ) ;
#23379 = EDGE_CURVE ( 'NONE', #4603, #22094, #9502, .T. ) ;
#23380 = EDGE_CURVE ( 'NONE', #12572, #15709, #5368, .T. ) ;
#23381 = CARTESIAN_POINT ( 'NONE',  ( 140.0355749532205891, 37.61698748598766429, -2.775557561562891351E-14 ) ) ;
#23382 = VERTEX_POINT ( 'NONE', #10979 ) ;
#23383 = PLANE ( 'NONE',  #20045 ) ;
#23384 = CARTESIAN_POINT ( 'NONE',  ( 7.499999999999999112, -4.330127018922205195, -1.000000000000000888 ) ) ;
#23385 = ADVANCED_FACE ( 'NONE', ( #1872 ), #14580, .F. ) ;
#23386 = FACE_OUTER_BOUND ( 'NONE', #12289, .T. ) ;
#23387 = CARTESIAN_POINT ( 'NONE',  ( -146.4450000000000784, -494.4690652294807478, 30.00000000000641975 ) ) ;
#23388 = DIRECTION ( 'NONE',  ( -1.000000000000000000, 0.000000000000000000, 0.000000000000000000 ) ) ;
#23389 = FACE_BOUND ( 'NONE', #22296, .T. ) ;
#23390 = CARTESIAN_POINT ( 'NONE',  ( -283.4314821058793541, 271.7107452280322377, 145.6845057130645102 ) ) ;
#23391 = ORIENTED_EDGE ( 'NONE', *, *, #6658, .F. ) ;
#23392 = ORIENTED_EDGE ( 'NONE', *, *, #13203, .T. ) ;
#23393 = DIRECTION ( 'NONE',  ( 0.000000000000000000, -0.000000000000000000, 1.000000000000000000 ) ) ;
#23394 = AXIS2_PLACEMENT_3D ( 'NONE', #736, #15722, #12246 ) ;
#23395 = CARTESIAN_POINT ( 'NONE',  ( -4.232971792145048787E-15, -9.016621985895911351, -7.999704684617487516 ) ) ;
#23396 = DIRECTION ( 'NONE',  ( 1.000000000000000000, 0.000000000000000000, 0.000000000000000000 ) ) ;
#23397 = EDGE_LOOP ( 'NONE', ( #9288, #15891, #22857, #12510 ) ) ;
#23398 = DIRECTION ( 'NONE',  ( -1.000000000000000000, 1.408839003528726857E-14, 6.982962677686266711E-15 ) ) ;
#23399 = LINE ( 'NONE', #21021, #20342 ) ;
#23400 = ORIENTED_EDGE ( 'NONE', *, *, #16898, .T. ) ;
#23401 = CARTESIAN_POINT ( 'NONE',  ( 280.4976310729377360, 269.7223300543793698, 146.1079617568159961 ) ) ;
#23402 = CYLINDRICAL_SURFACE ( 'NONE', #15720, 35.00000000000000000 ) ;
#23403 = ORIENTED_EDGE ( 'NONE', *, *, #13629, .T. ) ;
#23404 = CARTESIAN_POINT ( 'NONE',  ( -134.8618744214602714, -1076.402150461712608, -28.33934113061011217 ) ) ;
#23405 = CIRCLE ( 'NONE', #12260, 2.649999999999971934 ) ;
#23406 = VERTEX_POINT ( 'NONE', #3563 ) ;
#23407 = DIRECTION ( 'NONE',  ( 0.000000000000000000, 0.000000000000000000, -1.000000000000000000 ) ) ;
#23408 = FACE_OUTER_BOUND ( 'NONE', #19691, .T. ) ;
#23409 = ORIENTED_EDGE ( 'NONE', *, *, #11219, .F. ) ;
#23410 = ORIENTED_EDGE ( 'NONE', *, *, #19305, .F. ) ;
#23411 = DIRECTION ( 'NONE',  ( 5.758888509154132365E-17, 0.7071067811865489050, 0.7071067811865462405 ) ) ;
#23412 = EDGE_CURVE ( 'NONE', #9258, #12339, #21937, .T. ) ;
#23413 = APPLICATION_PROTOCOL_DEFINITION ( 'draft international standard', 'automotive_design', 1998, #8601 ) ;
#23414 = CARTESIAN_POINT ( 'NONE',  ( -281.0570750465943775, 270.1062614524586820, -149.6728700860324750 ) ) ;
#23415 = DIRECTION ( 'NONE',  ( -0.000000000000000000, -0.000000000000000000, 1.000000000000000000 ) ) ;
#23416 = DIRECTION ( 'NONE',  ( 0.000000000000000000, 0.000000000000000000, 1.000000000000000000 ) ) ;
#23417 = EDGE_LOOP ( 'NONE', ( #17667, #7038, #5972, #15809 ) ) ;
#23418 = CARTESIAN_POINT ( 'NONE',  ( 5.000000000000002665, 3.306546357697854226E-16, 2.700000000000000622 ) ) ;
#23419 = AXIS2_PLACEMENT_3D ( 'NONE', #2265, #11857, #20739 ) ;
#23420 = ORIENTED_EDGE ( 'NONE', *, *, #1307, .T. ) ;
#23421 = AXIS2_PLACEMENT_3D ( 'NONE', #9967, #9846, #654 ) ;
#23422 = TOROIDAL_SURFACE ( 'NONE', #11515, 22.50000000000000000, 1.500000000000000444 ) ;
#23423 = ORIENTED_EDGE ( 'NONE', *, *, #22635, .T. ) ;
#23424 = CARTESIAN_POINT ( 'NONE',  ( -123.1824219776881790, 83.04955713735581924, -32.49999999999356959 ) ) ;
#23425 = ORIENTED_EDGE ( 'NONE', *, *, #2389, .T. ) ;
#23426 = DIRECTION ( 'NONE',  ( 0.000000000000000000, 0.000000000000000000, 1.000000000000000000 ) ) ;
#23427 = ORIENTED_EDGE ( 'NONE', *, *, #23380, .T. ) ;
#23428 = CARTESIAN_POINT ( 'NONE',  ( 10.00000000000000000, 0.000000000000000000, 20.00000000000000000 ) ) ;
#23429 = ORIENTED_EDGE ( 'NONE', *, *, #9516, .T. ) ;
#23430 = EDGE_CURVE ( 'NONE', #5897, #12526, #22020, .T. ) ;
#23431 = CYLINDRICAL_SURFACE ( 'NONE', #2, 145.0000000000000284 ) ;
#23432 = VECTOR ( 'NONE', #15373, 1000.000000000000000 ) ;
#23433 =( LENGTH_UNIT ( ) NAMED_UNIT ( * ) SI_UNIT ( .MILLI., .METRE. ) );
#23434 = EDGE_CURVE ( 'NONE', #18342, #5818, #10389, .T. ) ;
#23435 = CONICAL_SURFACE ( 'NONE', #7629, 2.041999999999999815, 1.047197551196591858 ) ;
#23436 = LINE ( 'NONE', #18014, #16146 ) ;
#23437 = PLANE ( 'NONE',  #22714 ) ;
#23438 = VECTOR ( 'NONE', #14421, 1000.000000000000000 ) ;
#23439 = CARTESIAN_POINT ( 'NONE',  ( -7.499999999999999112, 34.18698582794336716, -100.0000000000000000 ) ) ;
#23440 = ORIENTED_EDGE ( 'NONE', *, *, #3992, .F. ) ;
#23441 = DIRECTION ( 'NONE',  ( -6.753181414994864868E-15, 6.753181414994864868E-15, -1.000000000000000000 ) ) ;
#23442 =( REPRESENTATION_RELATIONSHIP ('NONE','NONE', #10127, #6236 ) REPRESENTATION_RELATIONSHIP_WITH_TRANSFORMATION ( #19841 )SHAPE_REPRESENTATION_RELATIONSHIP( ) );
#23443 = ADVANCED_FACE ( 'NONE', ( #9915 ), #22405, .T. ) ;
#23444 = EDGE_CURVE ( 'NONE', #4308, #5940, #723, .T. ) ;
#23446 = ORIENTED_EDGE ( 'NONE', *, *, #7623, .T. ) ;
#23445 = ORIENTED_EDGE ( 'NONE', *, *, #937, .F. ) ;
#23447 = CARTESIAN_POINT ( 'NONE',  ( 0.000000000000000000, 0.000000000000000000, 0.000000000000000000 ) ) ;
#23448 = CARTESIAN_POINT ( 'NONE',  ( 0.000000000000000000, -1.178949249685213863, 2.042000000000002924 ) ) ;
#23449 = FACE_OUTER_BOUND ( 'NONE', #15580, .T. ) ;
#23450 = DIRECTION ( 'NONE',  ( 0.000000000000000000, 0.000000000000000000, 1.000000000000000000 ) ) ;
#23451 = CYLINDRICAL_SURFACE ( 'NONE', #22203, 2.500000000000002220 ) ;
#23452 = EDGE_CURVE ( 'NONE', #8832, #13544, #12349, .T. ) ;
#23453 = AXIS2_PLACEMENT_3D ( 'NONE', #17308, #6667, #756 ) ;
#23454 = AXIS2_PLACEMENT_3D ( 'NONE', #13657, #9649, #13184 ) ;
#23455 = EDGE_LOOP ( 'NONE', ( #19451, #23168, #2155, #20127 ) ) ;
#23456 = AXIS2_PLACEMENT_3D ( 'NONE', #16712, #163, #14910 ) ;
#23457 = FACE_OUTER_BOUND ( 'NONE', #9648, .T. ) ;
#23458 = AXIS2_PLACEMENT_3D ( 'NONE', #8647, #3189, #2836 ) ;
#23459 = ORIENTED_EDGE ( 'NONE', *, *, #219, .T. ) ;
#23460 = LINE ( 'NONE', #9345, #10805 ) ;
#23461 = DIRECTION ( 'NONE',  ( 1.000000000000000000, 0.000000000000000000, 0.000000000000000000 ) ) ;
#23462 = VERTEX_POINT ( 'NONE', #1994 ) ;
#23463 = ORIENTED_EDGE ( 'NONE', *, *, #13098, .T. ) ;
#23464 = CARTESIAN_POINT ( 'NONE',  ( -129.2447185937758718, 85.56171376302411602, -29.18615827854497624 ) ) ;
#23465 = CARTESIAN_POINT ( 'NONE',  ( 0.000000000000000000, -132.2000000000000455, 7.703011046602857601E-15 ) ) ;
#23466 = ORIENTED_EDGE ( 'NONE', *, *, #8841, .T. ) ;
#23467 = CARTESIAN_POINT ( 'NONE',  ( 99.99999999999987210, -129.2000000000000455, 177.2000000000014097 ) ) ;
#23468 = CARTESIAN_POINT ( 'NONE',  ( 133.6263423143003877, 78.54310546248494518, 31.99235058689527733 ) ) ;
#23469 = DIRECTION ( 'NONE',  ( -0.000000000000000000, 0.000000000000000000, 1.000000000000000000 ) ) ;
#23470 = PRODUCT_DEFINITION_SHAPE ( 'NONE', 'NONE',  #23813 ) ;
#23471 = COLOUR_RGB ( '',0.8941176470588234615, 0.8941176470588234615, 0.8941176470588234615 ) ;
#23472 = CARTESIAN_POINT ( 'NONE',  ( 0.2500000000000002220, 0.000000000000000000, 2.081668171172168513E-14 ) ) ;
#23473 = AXIS2_PLACEMENT_3D ( 'NONE', #7799, #13393, #22636 ) ;
#23474 = CIRCLE ( 'NONE', #6959, 10.00000000000000000 ) ;
#23475 = CARTESIAN_POINT ( 'NONE',  ( -129.2206655591605511, -1072.408698320350595, 32.05500000000641592 ) ) ;
#23477 = CIRCLE ( 'NONE', #16170, 145.0000000000000284 ) ;
#23476 = CARTESIAN_POINT ( 'NONE',  ( 99.99999999999987210, -132.2000000000001023, -113.4834095219707848 ) ) ;
#23478 = EDGE_CURVE ( 'NONE', #12107, #21209, #7598, .T. ) ;
#23479 = AXIS2_PLACEMENT_3D ( 'NONE', #4922, #17721, #19880 ) ;
#23480 = DIRECTION ( 'NONE',  ( 0.000000000000000000, 0.000000000000000000, -1.000000000000000000 ) ) ;
#23481 = VECTOR ( 'NONE', #6069, 1000.000000000000000 ) ;
#23482 = EDGE_CURVE ( 'NONE', #15472, #11870, #13038, .T. ) ;
#23483 = EDGE_LOOP ( 'NONE', ( #2871, #22284, #6275, #18440 ) ) ;
#23484 = EDGE_CURVE ( 'NONE', #12455, #21824, #15072, .T. ) ;
#23485 = DIRECTION ( 'NONE',  ( 1.000000000000000000, 0.000000000000000000, 0.000000000000000000 ) ) ;
#23486 = CARTESIAN_POINT ( 'NONE',  ( 7.922281120364393914, -4.573931137438282057, -8.047472243342932430 ) ) ;
#23487 = AXIS2_PLACEMENT_3D ( 'NONE', #16266, #8776, #21445 ) ;
#23488 = ORIENTED_EDGE ( 'NONE', *, *, #1246, .F. ) ;
#23489 = EDGE_CURVE ( 'NONE', #18313, #6750, #12367, .T. ) ;
#23490 = FACE_OUTER_BOUND ( 'NONE', #22033, .T. ) ;
#23491 = CYLINDRICAL_SURFACE ( 'NONE', #15693, 20.00000000000000000 ) ;
#23492 = PRODUCT_RELATED_PRODUCT_CATEGORY ( 'part', '', ( #13866 ) ) ;
#23493 = EDGE_CURVE ( 'NONE', #23309, #14920, #18412, .T. ) ;
#23494 = CARTESIAN_POINT ( 'NONE',  ( -146.4450000000001069, -204.4690652294807194, 27.50000000000642331 ) ) ;
#23495 = AXIS2_PLACEMENT_3D ( 'NONE', #3993, #13237, #20430 ) ;
#23497 = CIRCLE ( 'NONE', #22328, 145.0000000000000284 ) ;
#23496 = PRESENTATION_LAYER_ASSIGNMENT (  '', '', ( #8859 ) ) ;
#23498 = CARTESIAN_POINT ( 'NONE',  ( -281.4928932188135491, -127.0000000000000568, 152.4000000000014268 ) ) ;
#23499 = AXIS2_PLACEMENT_3D ( 'NONE', #20469, #4162, #9742 ) ;
#23500 = LINE ( 'NONE', #7067, #6903 ) ;
#23501 = VECTOR ( 'NONE', #19855, 1000.000000000000000 ) ;
#23502 = CIRCLE ( 'NONE', #4219, 2.649999999999999467 ) ;
#23503 = EDGE_LOOP ( 'NONE', ( #15341, #4304, #873, #23569 ) ) ;
#23504 = CIRCLE ( 'NONE', #15017, 7.500000000000000888 ) ;
#23505 = AXIS2_PLACEMENT_3D ( 'NONE', #617, #17159, #18952 ) ;
#23506 = FACE_BOUND ( 'NONE', #7911, .T. ) ;
#23507 = ORIENTED_EDGE ( 'NONE', *, *, #2066, .F. ) ;
#23508 = CARTESIAN_POINT ( 'NONE',  ( 145.0000000000000284, -500.0000000000000000, 30.00000000000001421 ) ) ;
#23509 = DIRECTION ( 'NONE',  ( 0.000000000000000000, 0.000000000000000000, -1.000000000000000000 ) ) ;
#23510 = ORIENTED_EDGE ( 'NONE', *, *, #21284, .T. ) ;
#23511 = FACE_OUTER_BOUND ( 'NONE', #18768, .T. ) ;
#23512 = DIRECTION ( 'NONE',  ( 1.000000000000000000, 0.000000000000000000, 0.000000000000000000 ) ) ;
#23513 = CARTESIAN_POINT ( 'NONE',  ( 0.000000000000000000, 0.000000000000000000, 0.000000000000000000 ) ) ;
#23514 = CARTESIAN_POINT ( 'NONE',  ( 70.00000000000000000, -87.33333333333332860, 3.000000000000000000 ) ) ;
#23515 = CARTESIAN_POINT ( 'NONE',  ( 5.200000000000002842, 3.306546357697854226E-16, 2.700000000000000622 ) ) ;
#23516 = PLANE ( 'NONE',  #1498 ) ;
#23517 = CARTESIAN_POINT ( 'NONE',  ( 18.83467029480910426, 16.52066876451826971, 145.0000119999999697 ) ) ;
#23518 = ORIENTED_EDGE ( 'NONE', *, *, #19334, .F. ) ;
#23519 = VERTEX_POINT ( 'NONE', #20706 ) ;
#23521 = VECTOR ( 'NONE', #3865, 1000.000000000000000 ) ;
#23520 = AXIS2_PLACEMENT_3D ( 'NONE', #11676, #2801, #8147 ) ;
#23522 = CARTESIAN_POINT ( 'NONE',  ( -137.5000000000000000, -5.062647941322544249E-13, -90.00000000000000000 ) ) ;
#23523 = DIRECTION ( 'NONE',  ( -1.000000000000000000, -3.202566417187951028E-16, -6.405132834375902056E-16 ) ) ;
#23524 = STYLED_ITEM ( 'NONE', ( #11285 ), #7558 ) ;
#23525 = VECTOR ( 'NONE', #23683, 1000.000000000000000 ) ;
#23526 = EDGE_LOOP ( 'NONE', ( #3996, #727, #16699, #10349 ) ) ;
#23527 = AXIS2_PLACEMENT_3D ( 'NONE', #5407, #19887, #7442 ) ;
#23528 = CARTESIAN_POINT ( 'NONE',  ( 0.000000000000000000, 0.000000000000000000, 90.00000000000000000 ) ) ;
#23529 = CARTESIAN_POINT ( 'NONE',  ( -155.0000000000000284, -1000.000000000000000, 90.00000000000000000 ) ) ;
#23530 = EDGE_CURVE ( 'NONE', #7573, #18096, #4167, .T. ) ;
#23531 = EDGE_CURVE ( 'NONE', #21395, #4516, #22331, .T. ) ;
#23532 = ADVANCED_FACE ( 'NONE', ( #12077 ), #4662, .F. ) ;
#23533 = VERTEX_POINT ( 'NONE', #2361 ) ;
#23534 = CARTESIAN_POINT ( 'NONE',  ( 280.2488155364687827, 272.8646579186752774, 146.3610889986682935 ) ) ;
#23535 = DIRECTION ( 'NONE',  ( 0.000000000000000000, 0.000000000000000000, -1.000000000000000000 ) ) ;
#23536 = ORIENTED_EDGE ( 'NONE', *, *, #8240, .F. ) ;
#23537 = PLANE ( 'NONE',  #9847 ) ;
#23538 = ORIENTED_EDGE ( 'NONE', *, *, #12765, .F. ) ;
#23539 = DIRECTION ( 'NONE',  ( 1.000000000000000000, 0.000000000000000000, 0.000000000000000000 ) ) ;
#23540 = AXIS2_PLACEMENT_3D ( 'NONE', #15553, #19610, #10482 ) ;
#23541 = FACE_OUTER_BOUND ( 'NONE', #1649, .T. ) ;
#23543 = VECTOR ( 'NONE', #19264, 1000.000000000000000 ) ;
#23542 = CYLINDRICAL_SURFACE ( 'NONE', #9033, 2.500000000000002220 ) ;
#23544 = EDGE_LOOP ( 'NONE', ( #11997, #7178, #7201, #22587, #22014 ) ) ;
#23545 = ORIENTED_EDGE ( 'NONE', *, *, #17713, .F. ) ;
#23546 = DIRECTION ( 'NONE',  ( -1.000000000000000000, 1.408839003528726857E-14, 6.982962677686266711E-15 ) ) ;
#23547 = AXIS2_PLACEMENT_3D ( 'NONE', #8663, #13668, #1176 ) ;
#23548 = DIRECTION ( 'NONE',  ( 1.000000000000000000, -3.495664435217746987E-15, 0.000000000000000000 ) ) ;
#23549 = DIRECTION ( 'NONE',  ( -1.000000000000000000, 3.495664435217746987E-15, 0.000000000000000000 ) ) ;
#23550 = CARTESIAN_POINT ( 'NONE',  ( 2.500000000000002220, -2.357898499370430834, 3.469446951953614189E-15 ) ) ;
#23551 = DIRECTION ( 'NONE',  ( 3.469446951953614682E-16, -1.000000000000000000, 3.483493295888648978E-15 ) ) ;
#23552 = ORIENTED_EDGE ( 'NONE', *, *, #23379, .T. ) ;
#23553 = LINE ( 'NONE', #13942, #2945 ) ;
#23554 =( NAMED_UNIT ( * ) SI_UNIT ( $, .STERADIAN. ) SOLID_ANGLE_UNIT ( ) );
#23555 = EDGE_LOOP ( 'NONE', ( #11071, #2144, #21891, #21065 ) ) ;
#23556 = EDGE_CURVE ( 'NONE', #13791, #67, #3647, .T. ) ;
#23557 = PLANE ( 'NONE',  #17906 ) ;
#23558 = CARTESIAN_POINT ( 'NONE',  ( 25.00004926069054889, -1.642023387880738872, -145.0000000000000000 ) ) ;
#23559 = ORIENTED_EDGE ( 'NONE', *, *, #6954, .F. ) ;
#23560 = CYLINDRICAL_SURFACE ( 'NONE', #20642, 2.199999999999979750 ) ;
#23561 = ORIENTED_EDGE ( 'NONE', *, *, #7344, .F. ) ;
#23562 = LINE ( 'NONE', #21, #1332 ) ;
#23563 = ORIENTED_EDGE ( 'NONE', *, *, #12157, .T. ) ;
#23564 = CARTESIAN_POINT ( 'NONE',  ( -288.2000000000008981, 35.00000000000100897, 107.6499999999999631 ) ) ;
#23565 = CARTESIAN_POINT ( 'NONE',  ( -281.2447782964895282, 268.3743436287469422, 147.1433523009092994 ) ) ;
#23566 = DIRECTION ( 'NONE',  ( 0.000000000000000000, -1.000000000000000000, 1.287488025362403787E-15 ) ) ;
#23567 = CARTESIAN_POINT ( 'NONE',  ( 79.04925354955338435, -121.5574576620390843, 90.00000000000000000 ) ) ;
#23568 = DIRECTION ( 'NONE',  ( 0.000000000000000000, 0.000000000000000000, 1.000000000000000000 ) ) ;
#23569 = ORIENTED_EDGE ( 'NONE', *, *, #8678, .T. ) ;
#23570 = LINE ( 'NONE', #1591, #15347 ) ;
#23571 = ADVANCED_FACE ( 'NONE', ( #4300 ), #6918, .F. ) ;
#23572 = PRODUCT_DEFINITION_SHAPE ( 'NONE', 'NONE',  #23846 ) ;
#23574 = ORIENTED_EDGE ( 'NONE', *, *, #17560, .F. ) ;
#23573 = ORIENTED_EDGE ( 'NONE', *, *, #4181, .F. ) ;
#23575 = DIRECTION ( 'NONE',  ( -3.469446951953613794E-15, 3.469446951953612611E-15, 1.000000000000000000 ) ) ;
#23576 = DIRECTION ( 'NONE',  ( 1.000000000000000000, -0.000000000000000000, 6.982962677686266711E-15 ) ) ;
#23577 = LINE ( 'NONE', #6796, #13079 ) ;
#23578 = EDGE_LOOP ( 'NONE', ( #17588, #18552 ) ) ;
#23579 = EDGE_CURVE ( 'NONE', #9060, #12933, #15547, .T. ) ;
#23580 = CARTESIAN_POINT ( 'NONE',  ( 2.500000000000000000, -1.178949249685213863, 2.042000000000001148 ) ) ;
#23581 = ORIENTED_EDGE ( 'NONE', *, *, #16566, .F. ) ;
#23582 = EDGE_CURVE ( 'NONE', #6031, #7824, #9745, .T. ) ;
#23583 = CARTESIAN_POINT ( 'NONE',  ( 0.2500000000000002220, 0.000000000000000000, 2.081668171172168513E-14 ) ) ;
#23584 = VERTEX_POINT ( 'NONE', #10114 ) ;
#23585 = DIRECTION ( 'NONE',  ( 0.000000000000000000, 0.000000000000000000, 1.000000000000000000 ) ) ;
#23586 = CARTESIAN_POINT ( 'NONE',  ( 0.000000000000000000, -2.342598717236910488, -4.057499999999997442 ) ) ;
#23587 = EDGE_CURVE ( 'NONE', #13361, #14650, #2674, .T. ) ;
#23588 = ITEM_DEFINED_TRANSFORMATION ( 'NONE', 'NONE', #11,  #11210 ) ;
#23589 = ORIENTED_EDGE ( 'NONE', *, *, #11441, .T. ) ;
#23590 = ORIENTED_EDGE ( 'NONE', *, *, #7394, .F. ) ;
#23591 = FACE_OUTER_BOUND ( 'NONE', #7541, .T. ) ;
#23592 = ORIENTED_EDGE ( 'NONE', *, *, #10970, .F. ) ;
#23593 = DIRECTION ( 'NONE',  ( -1.000000000000000000, 0.000000000000000000, 0.000000000000000000 ) ) ;
#23594 = CARTESIAN_POINT ( 'NONE',  ( 133.2563391751588142, 79.16925799295282218, 32.37408494914630097 ) ) ;
#23595 = CARTESIAN_POINT ( 'NONE',  ( 4.000000000000000888, 0.8228435280416209752, -3.430609588141487976 ) ) ;
#23596 = LINE ( 'NONE', #7050, #19825 ) ;
#23597 = DIRECTION ( 'NONE',  ( -0.000000000000000000, -0.000000000000000000, 1.000000000000000000 ) ) ;
#23598 = CYLINDRICAL_SURFACE ( 'NONE', #10031, 145.0000000000000284 ) ;
#23599 = ORIENTED_EDGE ( 'NONE', *, *, #10844, .F. ) ;
#23600 = CARTESIAN_POINT ( 'NONE',  ( -7.499999999999999112, 0.3744244963005040061, 1.590163186312071526E-15 ) ) ;
#23601 = CARTESIAN_POINT ( 'NONE',  ( -3.455068668934486276, 2.624017327439035707, -3.316620875263955437 ) ) ;
#23602 = ORIENTED_EDGE ( 'NONE', *, *, #9791, .F. ) ;
#23603 = CARTESIAN_POINT ( 'NONE',  ( -282.2000000000006708, 90.00000000000102318, -35.00000000000001421 ) ) ;
#23604 = CARTESIAN_POINT ( 'NONE',  ( 0.000000000000000000, 2.342598717236912709, 4.057499999999995666 ) ) ;
#23605 = AXIS2_PLACEMENT_3D ( 'NONE', #7571, #22060, #12938 ) ;
#23606 = CARTESIAN_POINT ( 'NONE',  ( -281.3520027839448971, 269.5592670532759030, 145.6220388411722695 ) ) ;
#23607 = ADVANCED_FACE ( 'NONE', ( #17100 ), #15659, .F. ) ;
#23608 = CARTESIAN_POINT ( 'NONE',  ( 9.999999999999998224, 6.123233995736764310E-16, 200.0000060000000133 ) ) ;
#23609 = DIRECTION ( 'NONE',  ( -1.000000000000000000, -0.000000000000000000, -0.000000000000000000 ) ) ;
#23610 = EDGE_CURVE ( 'NONE', #6626, #15256, #13914, .T. ) ;
#23611 = EDGE_LOOP ( 'NONE', ( #16176, #19423 ) ) ;
#23612 = CYLINDRICAL_SURFACE ( 'NONE', #19656, 145.0000000000000284 ) ;
#23613 = EDGE_CURVE ( 'NONE', #21765, #16976, #11943, .T. ) ;
#23614 = ORIENTED_EDGE ( 'NONE', *, *, #8900, .T. ) ;
#23615 = CARTESIAN_POINT ( 'NONE',  ( 287.4000000000013415, -129.2000000000000455, 146.4928932188134638 ) ) ;
#23616 = DIRECTION ( 'NONE',  ( 0.000000000000000000, 0.000000000000000000, 1.000000000000000000 ) ) ;
#23617 = SURFACE_SIDE_STYLE ('',( #16147 ) ) ;
#23618 = ORIENTED_EDGE ( 'NONE', *, *, #1633, .T. ) ;
#23619 = DIRECTION ( 'NONE',  ( 0.000000000000000000, -1.000000000000000000, 1.287488025362403787E-15 ) ) ;
#23620 = ADVANCED_FACE ( 'NONE', ( #13751 ), #13643, .F. ) ;
#23621 = CARTESIAN_POINT ( 'NONE',  ( 0.000000000000000000, -2.357898499370430834, 3.469446951953614189E-15 ) ) ;
#23622 = DIRECTION ( 'NONE',  ( -0.000000000000000000, -0.000000000000000000, 1.000000000000000000 ) ) ;
#23623 = DIRECTION ( 'NONE',  ( 0.000000000000000000, 0.000000000000000000, 1.000000000000000000 ) ) ;
#23624 = DIRECTION ( 'NONE',  ( 0.000000000000000000, -1.000000000000000000, 0.000000000000000000 ) ) ;
#23625 = FACE_OUTER_BOUND ( 'NONE', #11606, .T. ) ;
#23626 = DIRECTION ( 'NONE',  ( -1.000000000000000000, -0.000000000000000000, -0.000000000000000000 ) ) ;
#23627 = AXIS2_PLACEMENT_3D ( 'NONE', #10283, #16070, #23416 ) ;
#23628 = ORIENTED_EDGE ( 'NONE', *, *, #10968, .T. ) ;
#23629 = ORIENTED_EDGE ( 'NONE', *, *, #19153, .T. ) ;
#23630 = CYLINDRICAL_SURFACE ( 'NONE', #19968, 2.100000000000000089 ) ;
#23631 = DIRECTION ( 'NONE',  ( -1.000000000000000000, -0.000000000000000000, -0.000000000000000000 ) ) ;
#23632 = ORIENTED_EDGE ( 'NONE', *, *, #2683, .T. ) ;
#23633 = CARTESIAN_POINT ( 'NONE',  ( -129.2206655591611764, -1072.408698320350140, -29.99999999999356604 ) ) ;
#23634 = CARTESIAN_POINT ( 'NONE',  ( -146.0000000000000853, -784.4690652294805204, 30.00000000000641620 ) ) ;
#23635 = ORIENTED_EDGE ( 'NONE', *, *, #9886, .F. ) ;
#23636 = DIRECTION ( 'NONE',  ( 0.000000000000000000, -1.000000000000000000, 0.000000000000000000 ) ) ;
#23638 = CARTESIAN_POINT ( 'NONE',  ( 0.000000000000000000, 0.000000000000000000, -90.00000000000000000 ) ) ;
#23637 = B_SPLINE_CURVE_WITH_KNOTS ( 'NONE', 3,
 ( #8246, #23318, #22839, #15512, #23077, #2901, #15621, #13961, #4853, #4375 ),
 .UNSPECIFIED., .F., .F.,
 ( 4, 2, 2, 2, 4 ),
 ( 0.000000000000000000, 0.002305503304226491634, 0.004611006608452983269, 0.006916509912679474036, 0.009222013216905963068 ),
 .UNSPECIFIED. ) ;
#23639 = ORIENTED_EDGE ( 'NONE', *, *, #10221, .T. ) ;
#23640 = EDGE_CURVE ( 'NONE', #13636, #3749, #16802, .T. ) ;
#23641 = CIRCLE ( 'NONE', #7838, 2.500000000000002220 ) ;
#23642 = CARTESIAN_POINT ( 'NONE',  ( -44.99999999999995026, -52.79999999999969162, 52.65000000000018332 ) ) ;
#23643 = AXIS2_PLACEMENT_3D ( 'NONE', #20708, #19010, #14946 ) ;
#23644 = ORIENTED_EDGE ( 'NONE', *, *, #17526, .T. ) ;
#23645 = CARTESIAN_POINT ( 'NONE',  ( -44.80746418436748968, 137.9031948627972781, -90.00000000000000000 ) ) ;
#23646 = CARTESIAN_POINT ( 'NONE',  ( -129.6400180686264605, -1072.557589128678728, 32.50000000000641620 ) ) ;
#23647 = ORIENTED_EDGE ( 'NONE', *, *, #1439, .F. ) ;
#23648 = ORIENTED_EDGE ( 'NONE', *, *, #8122, .F. ) ;
#23649 = CARTESIAN_POINT ( 'NONE',  ( 282.6339272673396863, 272.3699028110927429, -145.4976310729377644 ) ) ;
#23650 = DIRECTION ( 'NONE',  ( 1.224646799147352961E-16, -7.087422195345027939E-32, 1.000000000000000000 ) ) ;
#23651 = CARTESIAN_POINT ( 'NONE',  ( -126.6511612778951132, 89.35598455390456252, -31.25955389945143281 ) ) ;
#23652 = ADVANCED_FACE ( 'NONE', ( #7801 ), #798, .F. ) ;
#23653 = EDGE_CURVE ( 'NONE', #1928, #21308, #17458, .T. ) ;
#23654 = DIRECTION ( 'NONE',  ( 1.000000000000000000, 0.000000000000000000, -0.000000000000000000 ) ) ;
#23655 = FACE_OUTER_BOUND ( 'NONE', #20992, .T. ) ;
#23656 = VERTEX_POINT ( 'NONE', #22637 ) ;
#23657 = LINE ( 'NONE', #1677, #8769 ) ;
#23658 = SURFACE_STYLE_USAGE ( .BOTH. , #18647 ) ;
#23659 = B_SPLINE_CURVE_WITH_KNOTS ( 'NONE', 3,
 ( #6052, #15501, #9252, #22589, #8233, #21026, #7533, #6296, #19202 ),
 .UNSPECIFIED., .F., .F.,
 ( 4, 2, 1, 2, 4 ),
 ( 0.000000000000000000, 0.002165063509461097498, 0.004330127018922194995, 0.006495190528383292493, 0.008660254037844389990 ),
 .UNSPECIFIED. ) ;
#23660 = FACE_OUTER_BOUND ( 'NONE', #5220, .T. ) ;
#23661 = CARTESIAN_POINT ( 'NONE',  ( 0.000000000000000000, -1000.000000000000000, -90.00000000000000000 ) ) ;
#23662 = VERTEX_POINT ( 'NONE', #6108 ) ;
#23663 = DIRECTION ( 'NONE',  ( -0.000000000000000000, -0.000000000000000000, 1.000000000000000000 ) ) ;
#23664 = AXIS2_PLACEMENT_3D ( 'NONE', #9320, #7600, #5674 ) ;
#23665 = EDGE_LOOP ( 'NONE', ( #22591, #15423, #18325, #2198 ) ) ;
#23666 = PRODUCT ( 'bucket', 'bucket', '', ( #3706 ) ) ;
#23667 = CIRCLE ( 'NONE', #10194, 5.249999999999956479 ) ;
#23668 = DIRECTION ( 'NONE',  ( -1.000000000000000000, -0.000000000000000000, -0.000000000000000000 ) ) ;
#23669 = ORIENTED_EDGE ( 'NONE', *, *, #9577, .T. ) ;
#23670 = FACE_OUTER_BOUND ( 'NONE', #2095, .T. ) ;
#23671 = ADVANCED_FACE ( 'NONE', ( #13528 ), #672, .F. ) ;
#23672 = LINE ( 'NONE', #21857, #15748 ) ;
#23673 = CARTESIAN_POINT ( 'NONE',  ( 125.8137507114119558, -1090.531233726929941, -31.11299551804367880 ) ) ;
#23674 = EDGE_CURVE ( 'NONE', #6206, #19753, #2285, .T. ) ;
#23675 = DIRECTION ( 'NONE',  ( -1.000000000000000000, 0.000000000000000000, -0.000000000000000000 ) ) ;
#23676 = ORIENTED_EDGE ( 'NONE', *, *, #10326, .F. ) ;
#23677 = CARTESIAN_POINT ( 'NONE',  ( -117.3074641843675749, 85.22886158240835641, -90.00000000000000000 ) ) ;
#23678 = SURFACE_STYLE_FILL_AREA ( #12752 ) ;
#23680 = ORIENTED_EDGE ( 'NONE', *, *, #18706, .T. ) ;
#23679 = ORIENTED_EDGE ( 'NONE', *, *, #15527, .T. ) ;
#23681 = AXIS2_PLACEMENT_3D ( 'NONE', #14097, #19853, #5020 ) ;
#23682 = DIRECTION ( 'NONE',  ( 0.000000000000000000, 0.000000000000000000, 1.000000000000000000 ) ) ;
#23683 = DIRECTION ( 'NONE',  ( -0.000000000000000000, 1.000000000000000000, -0.000000000000000000 ) ) ;
#23684 = DIRECTION ( 'NONE',  ( -1.000000000000000000, 0.000000000000000000, 0.000000000000000000 ) ) ;
#23685 = AXIS2_PLACEMENT_3D ( 'NONE', #17973, #16295, #23636 ) ;
#23686 = EDGE_LOOP ( 'NONE', ( #23079, #17574, #4352, #9274 ) ) ;
#23687 = CARTESIAN_POINT ( 'NONE',  ( 0.000000000000000000, -1000.000000000000000, -138.9999999999999716 ) ) ;
#23688 = CARTESIAN_POINT ( 'NONE',  ( -280.0000000000000568, 269.9999999999999432, -144.9999999999999716 ) ) ;
#23689 = ORIENTED_EDGE ( 'NONE', *, *, #12887, .T. ) ;
#23690 = CARTESIAN_POINT ( 'NONE',  ( 145.9999999999998295, -801.0618695410399823, 27.94500000000641649 ) ) ;
#23691 = CARTESIAN_POINT ( 'NONE',  ( 119.6158142514525622, -1087.367367941136990, -29.99999999999356604 ) ) ;
#23692 = EDGE_CURVE ( 'NONE', #22099, #22022, #17564, .T. ) ;
#23693 = ORIENTED_EDGE ( 'NONE', *, *, #7707, .T. ) ;
#23694 = ORIENTED_EDGE ( 'NONE', *, *, #20200, .F. ) ;
#23695 = EDGE_CURVE ( 'NONE', #326, #19241, #10711, .T. ) ;
#23696 = AXIS2_PLACEMENT_3D ( 'NONE', #9792, #5810, #16904 ) ;
#23697 = DIRECTION ( 'NONE',  ( 3.469446951953614682E-16, -1.000000000000000000, 3.483493295888648978E-15 ) ) ;
#23698 = ORIENTED_EDGE ( 'NONE', *, *, #7707, .F. ) ;
#23699 = CARTESIAN_POINT ( 'NONE',  ( 2.500000000000000000, 2.357898499370433054, -1.951563910473907981E-15 ) ) ;
#23700 = DIRECTION ( 'NONE',  ( -1.000000000000000000, -0.000000000000000000, -0.000000000000000000 ) ) ;
#23701 = AXIS2_PLACEMENT_3D ( 'NONE', #7373, #10911, #5207 ) ;
#23702 = CARTESIAN_POINT ( 'NONE',  ( 4.000000000000000000, 2.512223110932545023, -3.469391141908803711 ) ) ;
#23703 = AXIS2_PLACEMENT_3D ( 'NONE', #8295, #683, #15446 ) ;
#23704 = EDGE_CURVE ( 'NONE', #20959, #13509, #15772, .T. ) ;
#23705 = DIRECTION ( 'NONE',  ( 0.000000000000000000, -1.177509268541832635E-16, 1.000000000000000000 ) ) ;
#23706 = CARTESIAN_POINT ( 'NONE',  ( -44.99999999999995026, -56.79999999999969162, 52.65000000000019753 ) ) ;
#23707 = ORIENTED_EDGE ( 'NONE', *, *, #8447, .F. ) ;
#23708 = CYLINDRICAL_SURFACE ( 'NONE', #10359, 20.00000000000000000 ) ;
#23709 = CIRCLE ( 'NONE', #7133, 7.500000000000001776 ) ;
#23710 = DIRECTION ( 'NONE',  ( 0.000000000000000000, 0.000000000000000000, -1.000000000000000000 ) ) ;
#23711 = EDGE_CURVE ( 'NONE', #6064, #16055, #10426, .T. ) ;
#23712 =( REPRESENTATION_RELATIONSHIP ('NONE','NONE', #10127, #6508 ) REPRESENTATION_RELATIONSHIP_WITH_TRANSFORMATION ( #21183 )SHAPE_REPRESENTATION_RELATIONSHIP( ) );
#23713 = ORIENTED_EDGE ( 'NONE', *, *, #3250, .F. ) ;
#23714 = AXIS2_PLACEMENT_3D ( 'NONE', #22059, #5523, #16403 ) ;
#23715 = CARTESIAN_POINT ( 'NONE',  ( 280.6225751257470620, 269.5484459290826180, -146.3429506979392443 ) ) ;
#23716 = DIRECTION ( 'NONE',  ( 1.000000000000000000, 0.000000000000000000, 0.000000000000000000 ) ) ;
#23717 = CARTESIAN_POINT ( 'NONE',  ( 65.00000000000005684, -56.79999999999970584, 35.00000000000019185 ) ) ;
#23718 = VECTOR ( 'NONE', #2465, 1000.000000000000000 ) ;
#23719 = FACE_OUTER_BOUND ( 'NONE', #6536, .T. ) ;
#23720 = CARTESIAN_POINT ( 'NONE',  ( 280.6228333615949282, 271.9320353020573293, -148.1755088701071941 ) ) ;
#23721 = ORIENTED_EDGE ( 'NONE', *, *, #3975, .F. ) ;
#23722 = DIRECTION ( 'NONE',  ( 1.000000000000000000, 0.000000000000000000, 0.000000000000000000 ) ) ;
#23723 = VERTEX_POINT ( 'NONE', #3073 ) ;
#23724 = LINE ( 'NONE', #9264, #21048 ) ;
#23725 = CARTESIAN_POINT ( 'NONE',  ( -155.0000000000000284, -494.4690652294799520, -32.49999999999350564 ) ) ;
#23726 = AXIS2_PLACEMENT_3D ( 'NONE', #18999, #9735, #9492 ) ;
#23727 = ORIENTED_EDGE ( 'NONE', *, *, #18284, .F. ) ;
#23728 = CARTESIAN_POINT ( 'NONE',  ( 158.0000000000000284, -500.0000000000000000, -27.34999999999998721 ) ) ;
#23729 = CARTESIAN_POINT ( 'NONE',  ( 123.8014913250395921, -1093.264216588539966, -32.24959887471653985 ) ) ;
#23730 = ADVANCED_FACE ( 'NONE', ( #18050 ), #4888, .F. ) ;
#23731 = AXIS2_PLACEMENT_3D ( 'NONE', #18940, #240, #13314 ) ;
#23732 = CARTESIAN_POINT ( 'NONE',  ( 7.703011046602857601E-15, -132.2000000000000455, -146.4928932188134070 ) ) ;
#23733 = CARTESIAN_POINT ( 'NONE',  ( 60.00000000000000000, -61.99999999999999289, 3.000000000000000000 ) ) ;
#23734 = EDGE_CURVE ( 'NONE', #13071, #19884, #19099, .T. ) ;
#23735 = FACE_OUTER_BOUND ( 'NONE', #15750, .T. ) ;
#23736 = LINE ( 'NONE', #1534, #16538 ) ;
#23737 = DIRECTION ( 'NONE',  ( 1.000000000000000000, 0.000000000000000000, 0.000000000000000000 ) ) ;
#23738 = ORIENTED_EDGE ( 'NONE', *, *, #3538, .F. ) ;
#23739 = VERTEX_POINT ( 'NONE', #1497 ) ;
#23740 = FACE_BOUND ( 'NONE', #16333, .T. ) ;
#23741 = CARTESIAN_POINT ( 'NONE',  ( 232.0000000000000284, -490.0000000000001137, -56.99999999999996447 ) ) ;
#23742 = EDGE_CURVE ( 'NONE', #7880, #12455, #14657, .T. ) ;
#23743 = EDGE_LOOP ( 'NONE', ( #17143, #23592, #8036, #4631 ) ) ;
#23744 = EDGE_CURVE ( 'NONE', #11081, #13199, #1518, .T. ) ;
#23745 = DIRECTION ( 'NONE',  ( -1.000000000000000000, 1.408839003528726857E-14, 6.982962677686266711E-15 ) ) ;
#23746 = CARTESIAN_POINT ( 'NONE',  ( 5.276498195232308674, -6.073236878017951312, -7.633618187056764981 ) ) ;
#23747 = VECTOR ( 'NONE', #21902, 1000.000000000000000 ) ;
#23748 = ORIENTED_EDGE ( 'NONE', *, *, #17229, .F. ) ;
#23749 = CARTESIAN_POINT ( 'NONE',  ( 280.6220388411721274, 269.5592670532759030, 146.3520027839448119 ) ) ;
#23750 = CARTESIAN_POINT ( 'NONE',  ( -93.00000000000000000, 3.000000000000308198, 129.9038105676659711 ) ) ;
#23751 = ADVANCED_FACE ( 'NONE', ( #1263 ), #23598, .T. ) ;
#23752 = ORIENTED_EDGE ( 'NONE', *, *, #14592, .T. ) ;
#23753 = CARTESIAN_POINT ( 'NONE',  ( 117.3074641843682144, -85.22886158240748955, 90.00000000000000000 ) ) ;
#23754 = CARTESIAN_POINT ( 'NONE',  ( -65.00000000000000000, -52.79999999999933635, 155.0000000000001421 ) ) ;
#23755 = EDGE_LOOP ( 'NONE', ( #21091, #2485 ) ) ;
#23756 = CARTESIAN_POINT ( 'NONE',  ( 7.808623696107343193, 4.508310992947586193, -7.999704684617482187 ) ) ;
#23757 = DIRECTION ( 'NONE',  ( 1.000000000000000000, -3.495664435217746987E-15, -0.000000000000000000 ) ) ;
#23758 = CARTESIAN_POINT ( 'NONE',  ( -37.30746418436648071, -137.9031948627975908, -90.00000000000000000 ) ) ;
#23759 = EDGE_LOOP ( 'NONE', ( #5475, #18939, #8937, #1330 ) ) ;
#23760 = ORIENTED_EDGE ( 'NONE', *, *, #15372, .T. ) ;
#23761 = CARTESIAN_POINT ( 'NONE',  ( 0.000000000000000000, 0.000000000000000000, -4.000000000000000000 ) ) ;
#23762 = APPLICATION_PROTOCOL_DEFINITION ( 'draft international standard', 'automotive_design', 1998, #2750 ) ;
#23763 = CARTESIAN_POINT ( 'NONE',  ( 0.000000000000000000, -1.178949249685215417, 2.042000000000002036 ) ) ;
#23764 = CIRCLE ( 'NONE', #19922, 5.199999999999982414 ) ;
#23765 = FACE_OUTER_BOUND ( 'NONE', #20892, .T. ) ;
#23766 = CARTESIAN_POINT ( 'NONE',  ( 4.000000000000000000, -2.309401076758516691, -0.4999999999999995559 ) ) ;
#23767 = ORIENTED_EDGE ( 'NONE', *, *, #6506, .T. ) ;
#23768 = ADVANCED_FACE ( 'NONE', ( #5248 ), #21194, .F. ) ;
#23769 = CIRCLE ( 'NONE', #12637, 145.0000000000000284 ) ;
#23770 = EDGE_CURVE ( 'NONE', #11056, #8135, #4990, .T. ) ;
#23771 = EDGE_CURVE ( 'NONE', #1821, #2323, #8528, .T. ) ;
#23772 = EDGE_CURVE ( 'NONE', #6747, #12326, #18471, .T. ) ;
#23773 = AXIS2_PLACEMENT_3D ( 'NONE', #18485, #6948, #5023 ) ;
#23774 =( BOUNDED_SURFACE ( )  B_SPLINE_SURFACE ( 3, 2, ( 
 ( #1116, #8256, #19343 ),
 ( #22847, #17319, #768 ),
 ( #15743, #21293, #10093 ),
 ( #10453, #11914, #17432 ),
 ( #876, #17794, #6432 ),
 ( #23210, #8368, #14073 ),
 ( #8612, #2802, #8148 ),
 ( #15521, #21168, #4636 ) ),
 .UNSPECIFIED., .F., .F., .F. ) 
 B_SPLINE_SURFACE_WITH_KNOTS ( ( 4, 2, 2, 4 ),
 ( 3, 3 ),
 ( 0.03850042371095789562, 0.04313406099830585649, 0.04545087964197984387, 0.04776769828565382431 ),
 ( 0.000000000000000000, 1.000000000000000000 ),
 .UNSPECIFIED. ) 
 GEOMETRIC_REPRESENTATION_ITEM ( )  RATIONAL_B_SPLINE_SURFACE ( (
 ( 1.000000000000000000, 0.8047781847388135734, 1.000000000000000000),
 ( 1.000000000000000000, 0.8123760230793541925, 1.000000000000000000),
 ( 1.000000000000000000, 0.8190653851695529619, 1.000000000000000000),
 ( 1.000000000000000000, 0.8191940386278896424, 1.000000000000000000),
 ( 1.000000000000000000, 0.8176096570055705337, 1.000000000000000000),
 ( 1.000000000000000000, 0.8122964723277524834, 1.000000000000000000),
 ( 1.000000000000000000, 0.8086312464132844324, 1.000000000000000000),
 ( 1.000000000000000000, 0.8047712192439641088, 1.000000000000000000) ) ) 
 REPRESENTATION_ITEM ( '' )  SURFACE ( )  );
#23775 = DIRECTION ( 'NONE',  ( 0.000000000000000000, -0.4999999999999993339, 0.8660254037844390407 ) ) ;
#23776 = CARTESIAN_POINT ( 'NONE',  ( 30.00000000000000000, 0.000000000000000000, -6.938893903907228378E-15 ) ) ;
#23777 = EDGE_CURVE ( 'NONE', #8918, #5697, #4611, .T. ) ;
#23778 = ORIENTED_EDGE ( 'NONE', *, *, #9514, .T. ) ;
#23779 = CIRCLE ( 'NONE', #13044, 2.649999999999992806 ) ;
#23781 = EDGE_CURVE ( 'NONE', #506, #5068, #743, .T. ) ;
#23780 = CARTESIAN_POINT ( 'NONE',  ( 0.3306966981845720355, 8.469326210127405830, -7.349897473153450989 ) ) ;
#23782 = VERTEX_POINT ( 'NONE', #5022 ) ;
#23783 = CYLINDRICAL_SURFACE ( 'NONE', #7906, 20.00000000000000000 ) ;
#23784 = DIRECTION ( 'NONE',  ( -1.000000000000000000, 6.938893903907227392E-16, -2.425604463963772562E-30 ) ) ;
#23785 = EDGE_LOOP ( 'NONE', ( #5195, #20942, #4804, #17801 ) ) ;
#23786 = CARTESIAN_POINT ( 'NONE',  ( 0.6448876103708359731, 4.246476118072354922, -0.2256878752776725616 ) ) ;
#23787 = CARTESIAN_POINT ( 'NONE',  ( -18.83467029480908295, -1016.520668764518291, 145.0000119999999697 ) ) ;
#23788 = CIRCLE ( 'NONE', #9944, 145.0000000000000284 ) ;
#23789 = DIRECTION ( 'NONE',  ( 1.000000000000000000, 0.000000000000000000, 0.000000000000000000 ) ) ;
#23790 = DIRECTION ( 'NONE',  ( -0.000000000000000000, 1.000000000000000000, -3.469446951953613794E-15 ) ) ;
#23791 = LINE ( 'NONE', #7250, #19629 ) ;
#23792 = ORIENTED_EDGE ( 'NONE', *, *, #19188, .F. ) ;
#23793 = CARTESIAN_POINT ( 'NONE',  ( -285.2000000000014666, -127.0000000000000568, -146.4928932188134070 ) ) ;
#23794 = AXIS2_PLACEMENT_3D ( 'NONE', #11266, #18808, #5800 ) ;
#23795 = AXIS2_PLACEMENT_3D ( 'NONE', #20527, #7860, #20770 ) ;
#23797 = VERTEX_POINT ( 'NONE', #12430 ) ;
#23796 = ORIENTED_EDGE ( 'NONE', *, *, #1951, .F. ) ;
#23798 = DIRECTION ( 'NONE',  ( 1.000000000000000000, 0.000000000000000000, 0.000000000000000000 ) ) ;
#23799 = DIRECTION ( 'NONE',  ( -0.8191520442889902442, 0.000000000000000000, -0.5735764363510482688 ) ) ;
#23800 = CARTESIAN_POINT ( 'NONE',  ( 4.000000000000000000, 0.9868501483902631932, -0.09357334158579604100 ) ) ;
#23801 = ORIENTED_EDGE ( 'NONE', *, *, #2883, .T. ) ;
#23802 = DIRECTION ( 'NONE',  ( 0.000000000000000000, 0.000000000000000000, 1.000000000000000000 ) ) ;
#23803 = EDGE_CURVE ( 'NONE', #15819, #10120, #19731, .T. ) ;
#35 = AXIS2_PLACEMENT_3D ( 'NONE', #14341, #8390, #14444 ) ;
#23805 = NEXT_ASSEMBLY_USAGE_OCCURRENCE ( 'NAUO1', ' ', ' ', #20365, #21557, $ ) ;
#23806 = NEXT_ASSEMBLY_USAGE_OCCURRENCE ( 'NAUO2', ' ', ' ', #20365, #6213, $ ) ;
#23807 = NEXT_ASSEMBLY_USAGE_OCCURRENCE ( 'NAUO3', ' ', ' ', #20365, #11555, $ ) ;
#23808 = NEXT_ASSEMBLY_USAGE_OCCURRENCE ( 'NAUO4', ' ', ' ', #20365, #7979, $ ) ;
#23809 = NEXT_ASSEMBLY_USAGE_OCCURRENCE ( 'NAUO5', ' ', ' ', #20365, #14645, $ ) ;
#23810 = NEXT_ASSEMBLY_USAGE_OCCURRENCE ( 'NAUO6', ' ', ' ', #20365, #21557, $ ) ;
#23811 = NEXT_ASSEMBLY_USAGE_OCCURRENCE ( 'NAUO7', ' ', ' ', #20365, #6213, $ ) ;
#23812 = NEXT_ASSEMBLY_USAGE_OCCURRENCE ( 'NAUO8', ' ', ' ', #20365, #16409, $ ) ;
#23813 = NEXT_ASSEMBLY_USAGE_OCCURRENCE ( 'NAUO9', ' ', ' ', #20365, #16409, $ ) ;
#23814 = NEXT_ASSEMBLY_USAGE_OCCURRENCE ( 'NAUO10', ' ', ' ', #20365, #7979, $ ) ;
#23815 = NEXT_ASSEMBLY_USAGE_OCCURRENCE ( 'NAUO11', ' ', ' ', #20365, #7979, $ ) ;
#23816 = NEXT_ASSEMBLY_USAGE_OCCURRENCE ( 'NAUO12', ' ', ' ', #20365, #7979, $ ) ;
#23817 = NEXT_ASSEMBLY_USAGE_OCCURRENCE ( 'NAUO13', ' ', ' ', #20365, #7979, $ ) ;
#23818 = NEXT_ASSEMBLY_USAGE_OCCURRENCE ( 'NAUO14', ' ', ' ', #20365, #7979, $ ) ;
#23819 = NEXT_ASSEMBLY_USAGE_OCCURRENCE ( 'NAUO15', ' ', ' ', #20365, #7979, $ ) ;
#23820 = NEXT_ASSEMBLY_USAGE_OCCURRENCE ( 'NAUO16', ' ', ' ', #20365, #7979, $ ) ;
#23821 = NEXT_ASSEMBLY_USAGE_OCCURRENCE ( 'NAUO17', ' ', ' ', #20365, #7979, $ ) ;
#23822 = NEXT_ASSEMBLY_USAGE_OCCURRENCE ( 'NAUO18', ' ', ' ', #20365, #7979, $ ) ;
#23823 = NEXT_ASSEMBLY_USAGE_OCCURRENCE ( 'NAUO19', ' ', ' ', #20365, #16409, $ ) ;
#23824 = NEXT_ASSEMBLY_USAGE_OCCURRENCE ( 'NAUO20', ' ', ' ', #20365, #16409, $ ) ;
#23825 = NEXT_ASSEMBLY_USAGE_OCCURRENCE ( 'NAUO21', ' ', ' ', #20365, #16409, $ ) ;
#23826 = NEXT_ASSEMBLY_USAGE_OCCURRENCE ( 'NAUO22', ' ', ' ', #20365, #16409, $ ) ;
#23827 = NEXT_ASSEMBLY_USAGE_OCCURRENCE ( 'NAUO23', ' ', ' ', #20365, #16409, $ ) ;
#23828 = NEXT_ASSEMBLY_USAGE_OCCURRENCE ( 'NAUO24', ' ', ' ', #20365, #16409, $ ) ;
#23829 = NEXT_ASSEMBLY_USAGE_OCCURRENCE ( 'NAUO25', ' ', ' ', #20365, #16409, $ ) ;
#23830 = NEXT_ASSEMBLY_USAGE_OCCURRENCE ( 'NAUO26', ' ', ' ', #20365, #16409, $ ) ;
#23831 = NEXT_ASSEMBLY_USAGE_OCCURRENCE ( 'NAUO27', ' ', ' ', #20365, #16409, $ ) ;
#23832 = NEXT_ASSEMBLY_USAGE_OCCURRENCE ( 'NAUO28', ' ', ' ', #20365, #16409, $ ) ;
#23833 = NEXT_ASSEMBLY_USAGE_OCCURRENCE ( 'NAUO29', ' ', ' ', #20365, #16409, $ ) ;
#23834 = NEXT_ASSEMBLY_USAGE_OCCURRENCE ( 'NAUO30', ' ', ' ', #20365, #16409, $ ) ;
#23835 = NEXT_ASSEMBLY_USAGE_OCCURRENCE ( 'NAUO31', ' ', ' ', #20365, #16409, $ ) ;
#23836 = NEXT_ASSEMBLY_USAGE_OCCURRENCE ( 'NAUO32', ' ', ' ', #20365, #16409, $ ) ;
#23837 = NEXT_ASSEMBLY_USAGE_OCCURRENCE ( 'NAUO33', ' ', ' ', #20365, #16409, $ ) ;
#23838 = NEXT_ASSEMBLY_USAGE_OCCURRENCE ( 'NAUO34', ' ', ' ', #20365, #16409, $ ) ;
#23839 = NEXT_ASSEMBLY_USAGE_OCCURRENCE ( 'NAUO35', ' ', ' ', #20365, #16409, $ ) ;
#23840 = NEXT_ASSEMBLY_USAGE_OCCURRENCE ( 'NAUO36', ' ', ' ', #20365, #16409, $ ) ;
#23841 = NEXT_ASSEMBLY_USAGE_OCCURRENCE ( 'NAUO37', ' ', ' ', #20365, #9630, $ ) ;
#23842 = NEXT_ASSEMBLY_USAGE_OCCURRENCE ( 'NAUO38', ' ', ' ', #20365, #9630, $ ) ;
#23843 = NEXT_ASSEMBLY_USAGE_OCCURRENCE ( 'NAUO39', ' ', ' ', #20365, #9630, $ ) ;
#23844 = NEXT_ASSEMBLY_USAGE_OCCURRENCE ( 'NAUO40', ' ', ' ', #20365, #9630, $ ) ;
#23845 = NEXT_ASSEMBLY_USAGE_OCCURRENCE ( 'NAUO41', ' ', ' ', #20365, #2813, $ ) ;
#23846 = NEXT_ASSEMBLY_USAGE_OCCURRENCE ( 'NAUO42', ' ', ' ', #20365, #4601, $ ) ;
#23847 = NEXT_ASSEMBLY_USAGE_OCCURRENCE ( 'NAUO43', ' ', ' ', #20365, #17442, $ ) ;
#23848 = NEXT_ASSEMBLY_USAGE_OCCURRENCE ( 'NAUO44', ' ', ' ', #20365, #12164, $ ) ;
#23849 = NEXT_ASSEMBLY_USAGE_OCCURRENCE ( 'NAUO45', ' ', ' ', #20365, #19197, $ ) ;
#23850 = NEXT_ASSEMBLY_USAGE_OCCURRENCE ( 'NAUO46', ' ', ' ', #20365, #19197, $ ) ;
#23851 = NEXT_ASSEMBLY_USAGE_OCCURRENCE ( 'NAUO47', ' ', ' ', #20365, #19197, $ ) ;
#23852 = NEXT_ASSEMBLY_USAGE_OCCURRENCE ( 'NAUO48', ' ', ' ', #20365, #19197, $ ) ;
#23853 = NEXT_ASSEMBLY_USAGE_OCCURRENCE ( 'NAUO49', ' ', ' ', #20365, #16837, $ ) ;
#23854 = NEXT_ASSEMBLY_USAGE_OCCURRENCE ( 'NAUO50', ' ', ' ', #20365, #16837, $ ) ;
#23855 = NEXT_ASSEMBLY_USAGE_OCCURRENCE ( 'NAUO51', ' ', ' ', #20365, #16837, $ ) ;
#23856 = NEXT_ASSEMBLY_USAGE_OCCURRENCE ( 'NAUO52', ' ', ' ', #20365, #16837, $ ) ;
#23857 = NEXT_ASSEMBLY_USAGE_OCCURRENCE ( 'NAUO53', ' ', ' ', #20365, #20665, $ ) ;
#23858 = NEXT_ASSEMBLY_USAGE_OCCURRENCE ( 'NAUO54', ' ', ' ', #20365, #20665, $ ) ;
#23859 = NEXT_ASSEMBLY_USAGE_OCCURRENCE ( 'NAUO55', ' ', ' ', #20365, #20665, $ ) ;
#23860 = NEXT_ASSEMBLY_USAGE_OCCURRENCE ( 'NAUO56', ' ', ' ', #20365, #20665, $ ) ;
#23861 = NEXT_ASSEMBLY_USAGE_OCCURRENCE ( 'NAUO57', ' ', ' ', #20365, #16837, $ ) ;
#23862 = NEXT_ASSEMBLY_USAGE_OCCURRENCE ( 'NAUO58', ' ', ' ', #20365, #16837, $ ) ;
#23863 = NEXT_ASSEMBLY_USAGE_OCCURRENCE ( 'NAUO59', ' ', ' ', #20365, #16837, $ ) ;
#23864 = NEXT_ASSEMBLY_USAGE_OCCURRENCE ( 'NAUO60', ' ', ' ', #20365, #16837, $ ) ;
#23865 = NEXT_ASSEMBLY_USAGE_OCCURRENCE ( 'NAUO61', ' ', ' ', #20365, #5780, $ ) ;
#23866 = NEXT_ASSEMBLY_USAGE_OCCURRENCE ( 'NAUO62', ' ', ' ', #20365, #5780, $ ) ;
#23867 = NEXT_ASSEMBLY_USAGE_OCCURRENCE ( 'NAUO63', ' ', ' ', #20365, #16109, $ ) ;
#23868 = NEXT_ASSEMBLY_USAGE_OCCURRENCE ( 'NAUO64', ' ', ' ', #20365, #16109, $ ) ;
#23869 = NEXT_ASSEMBLY_USAGE_OCCURRENCE ( 'NAUO65', ' ', ' ', #20365, #1042, $ ) ;
#23870 = NEXT_ASSEMBLY_USAGE_OCCURRENCE ( 'NAUO66', ' ', ' ', #20365, #1042, $ ) ;
#23871 = NEXT_ASSEMBLY_USAGE_OCCURRENCE ( 'NAUO67', ' ', ' ', #20365, #1042, $ ) ;
#23872 = NEXT_ASSEMBLY_USAGE_OCCURRENCE ( 'NAUO68', ' ', ' ', #20365, #1042, $ ) ;
#23873 = NEXT_ASSEMBLY_USAGE_OCCURRENCE ( 'NAUO69', ' ', ' ', #20365, #1042, $ ) ;
#23874 = NEXT_ASSEMBLY_USAGE_OCCURRENCE ( 'NAUO70', ' ', ' ', #20365, #1042, $ ) ;
#23875 = NEXT_ASSEMBLY_USAGE_OCCURRENCE ( 'NAUO71', ' ', ' ', #20365, #1042, $ ) ;
#23876 = NEXT_ASSEMBLY_USAGE_OCCURRENCE ( 'NAUO72', ' ', ' ', #20365, #1042, $ ) ;
#23877 = NEXT_ASSEMBLY_USAGE_OCCURRENCE ( 'NAUO73', ' ', ' ', #20365, #16837, $ ) ;
#23878 = NEXT_ASSEMBLY_USAGE_OCCURRENCE ( 'NAUO74', ' ', ' ', #20365, #16837, $ ) ;
#23879 = NEXT_ASSEMBLY_USAGE_OCCURRENCE ( 'NAUO75', ' ', ' ', #20365, #16837, $ ) ;
#23880 = NEXT_ASSEMBLY_USAGE_OCCURRENCE ( 'NAUO76', ' ', ' ', #20365, #16837, $ ) ;
#23881 = NEXT_ASSEMBLY_USAGE_OCCURRENCE ( 'NAUO77', ' ', ' ', #20365, #16837, $ ) ;
#23882 = NEXT_ASSEMBLY_USAGE_OCCURRENCE ( 'NAUO78', ' ', ' ', #20365, #16837, $ ) ;
#23883 = NEXT_ASSEMBLY_USAGE_OCCURRENCE ( 'NAUO79', ' ', ' ', #20365, #16837, $ ) ;
#23884 = NEXT_ASSEMBLY_USAGE_OCCURRENCE ( 'NAUO80', ' ', ' ', #20365, #16837, $ ) ;
#23885 = NEXT_ASSEMBLY_USAGE_OCCURRENCE ( 'NAUO81', ' ', ' ', #20365, #5780, $ ) ;
#23886 = NEXT_ASSEMBLY_USAGE_OCCURRENCE ( 'NAUO82', ' ', ' ', #20365, #5780, $ ) ;
#23887 = NEXT_ASSEMBLY_USAGE_OCCURRENCE ( 'NAUO83', ' ', ' ', #20365, #16109, $ ) ;
#23888 = NEXT_ASSEMBLY_USAGE_OCCURRENCE ( 'NAUO84', ' ', ' ', #20365, #16109, $ ) ;
#23889 = NEXT_ASSEMBLY_USAGE_OCCURRENCE ( 'NAUO85', ' ', ' ', #20365, #5780, $ ) ;
#23890 = NEXT_ASSEMBLY_USAGE_OCCURRENCE ( 'NAUO86', ' ', ' ', #20365, #5780, $ ) ;
#23891 = NEXT_ASSEMBLY_USAGE_OCCURRENCE ( 'NAUO87', ' ', ' ', #20365, #16109, $ ) ;
#23892 = NEXT_ASSEMBLY_USAGE_OCCURRENCE ( 'NAUO88', ' ', ' ', #20365, #16109, $ ) ;
#23893=COLOUR_RGB('Dark Blue',0.08,0.2,0.34);
#23894=FILL_AREA_STYLE_COLOUR('',#23893);
#23895=FILL_AREA_STYLE('',(#23894));
#23896=SURFACE_STYLE_FILL_AREA(#23895);
#23897=SURFACE_SIDE_STYLE('',(#23896));
#23898=SURFACE_STYLE_USAGE(.BOTH.,#23897);
#23899=PRESENTATION_STYLE_ASSIGNMENT((#23898));
#23900=COLOUR_RGB('Light Blue',0.38,0.62,0.78);
#23901=FILL_AREA_STYLE_COLOUR('',#23900);
#23902=FILL_AREA_STYLE('',(#23901));
#23903=SURFACE_STYLE_FILL_AREA(#23902);
#23904=SURFACE_SIDE_STYLE('',(#23903));
#23905=SURFACE_STYLE_USAGE(.BOTH.,#23904);
#23906=PRESENTATION_STYLE_ASSIGNMENT((#23905));
#23907=COLOUR_RGB('Sky Blue',0.24,0.69,0.87);
#23908=FILL_AREA_STYLE_COLOUR('',#23907);
#23909=FILL_AREA_STYLE('',(#23908));
#23910=SURFACE_STYLE_FILL_AREA(#23909);
#23911=SURFACE_SIDE_STYLE('',(#23910));
#23912=SURFACE_STYLE_USAGE(.BOTH.,#23911);
#23913=PRESENTATION_STYLE_ASSIGNMENT((#23912));
#23914=COLOUR_RGB('Grey',0.48,0.52,0.57);
#23915=FILL_AREA_STYLE_COLOUR('',#23914);
#23916=FILL_AREA_STYLE('',(#23915));
#23917=SURFACE_STYLE_FILL_AREA(#23916);
#23918=SURFACE_SIDE_STYLE('',(#23917));
#23919=SURFACE_STYLE_USAGE(.BOTH.,#23918);
#23920=PRESENTATION_STYLE_ASSIGNMENT((#23919));
#23921=COLOUR_RGB('Black',0.12,0.14,0.17);
#23922=FILL_AREA_STYLE_COLOUR('',#23921);
#23923=FILL_AREA_STYLE('',(#23922));
#23924=SURFACE_STYLE_FILL_AREA(#23923);
#23925=SURFACE_SIDE_STYLE('',(#23924));
#23926=SURFACE_STYLE_USAGE(.BOTH.,#23925);
#23927=PRESENTATION_STYLE_ASSIGNMENT((#23926));
#23928=COLOUR_RGB('Off White',0.89,0.88,0.83);
#23929=FILL_AREA_STYLE_COLOUR('',#23928);
#23930=FILL_AREA_STYLE('',(#23929));
#23931=SURFACE_STYLE_FILL_AREA(#23930);
#23932=SURFACE_SIDE_STYLE('',(#23931));
#23933=SURFACE_STYLE_USAGE(.BOTH.,#23932);
#23934=PRESENTATION_STYLE_ASSIGNMENT((#23933));
ENDSEC;
END-ISO-10303-21;
